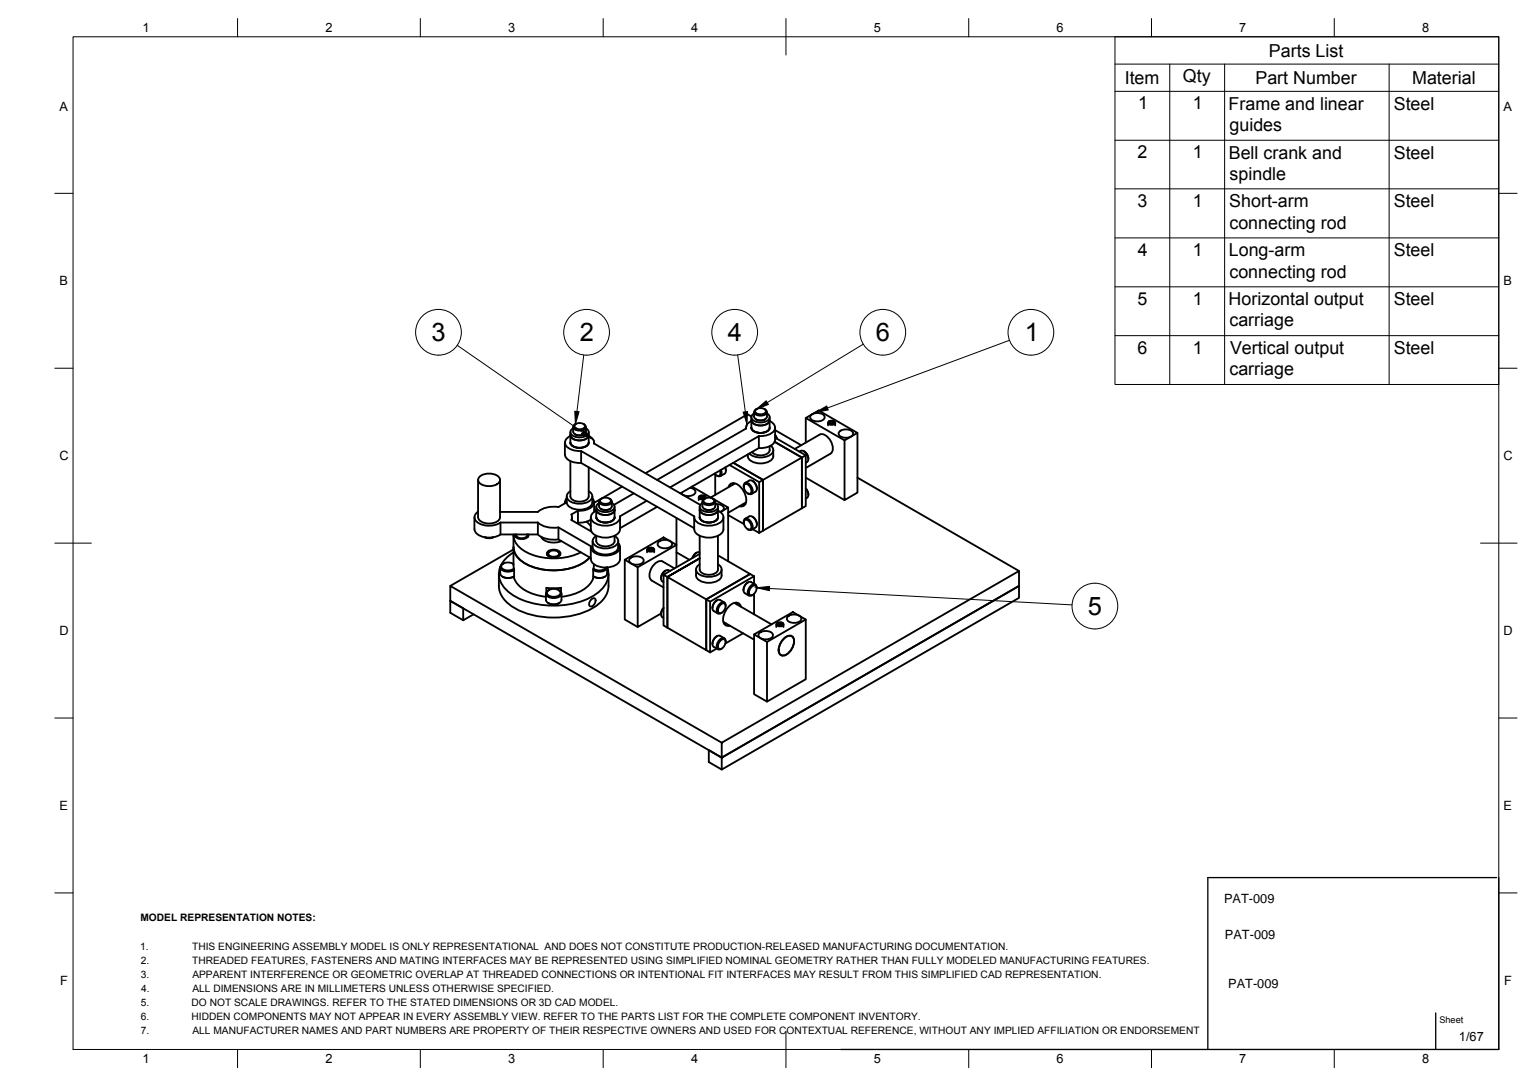
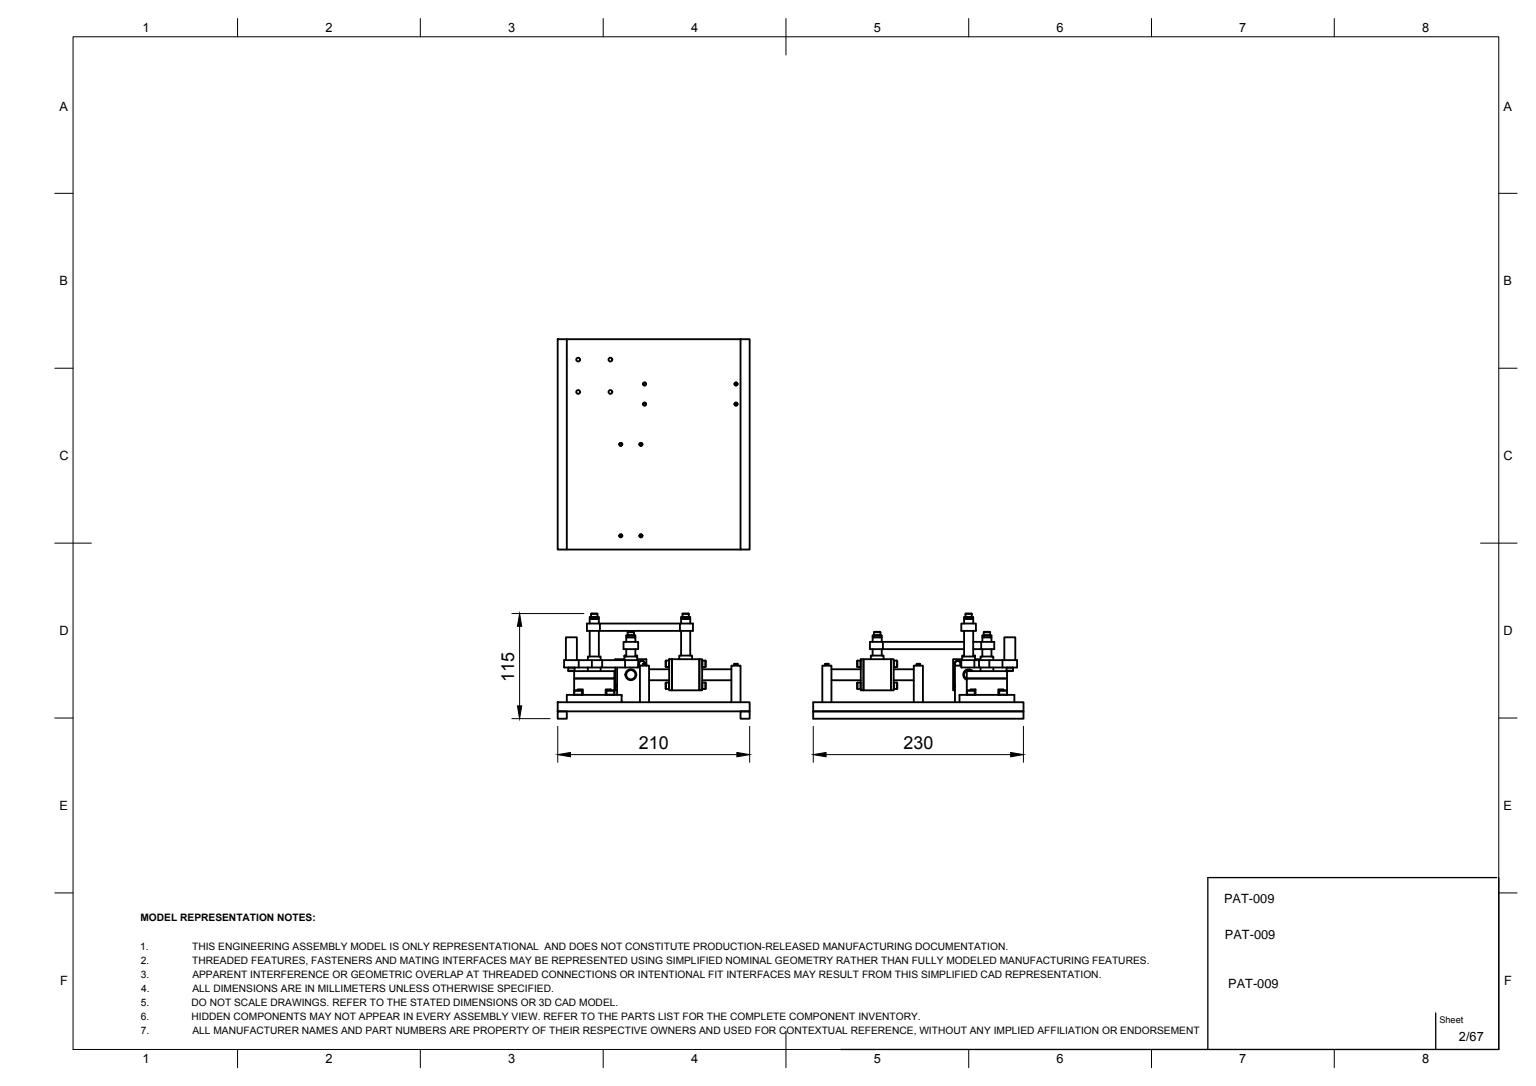
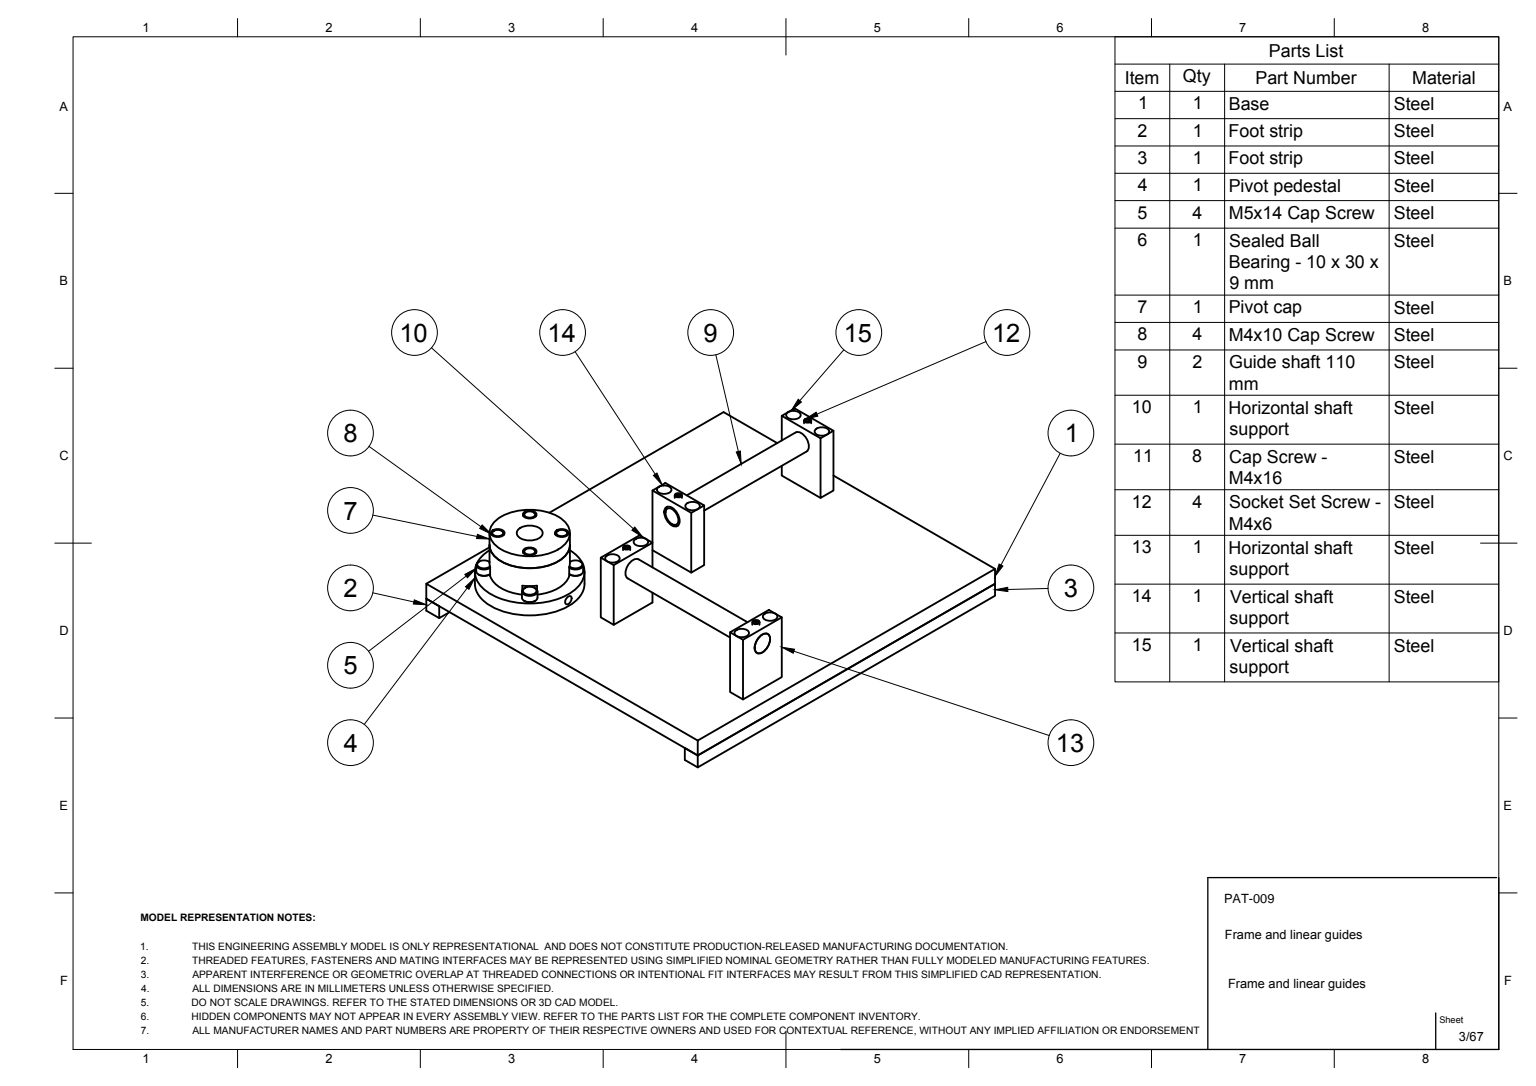
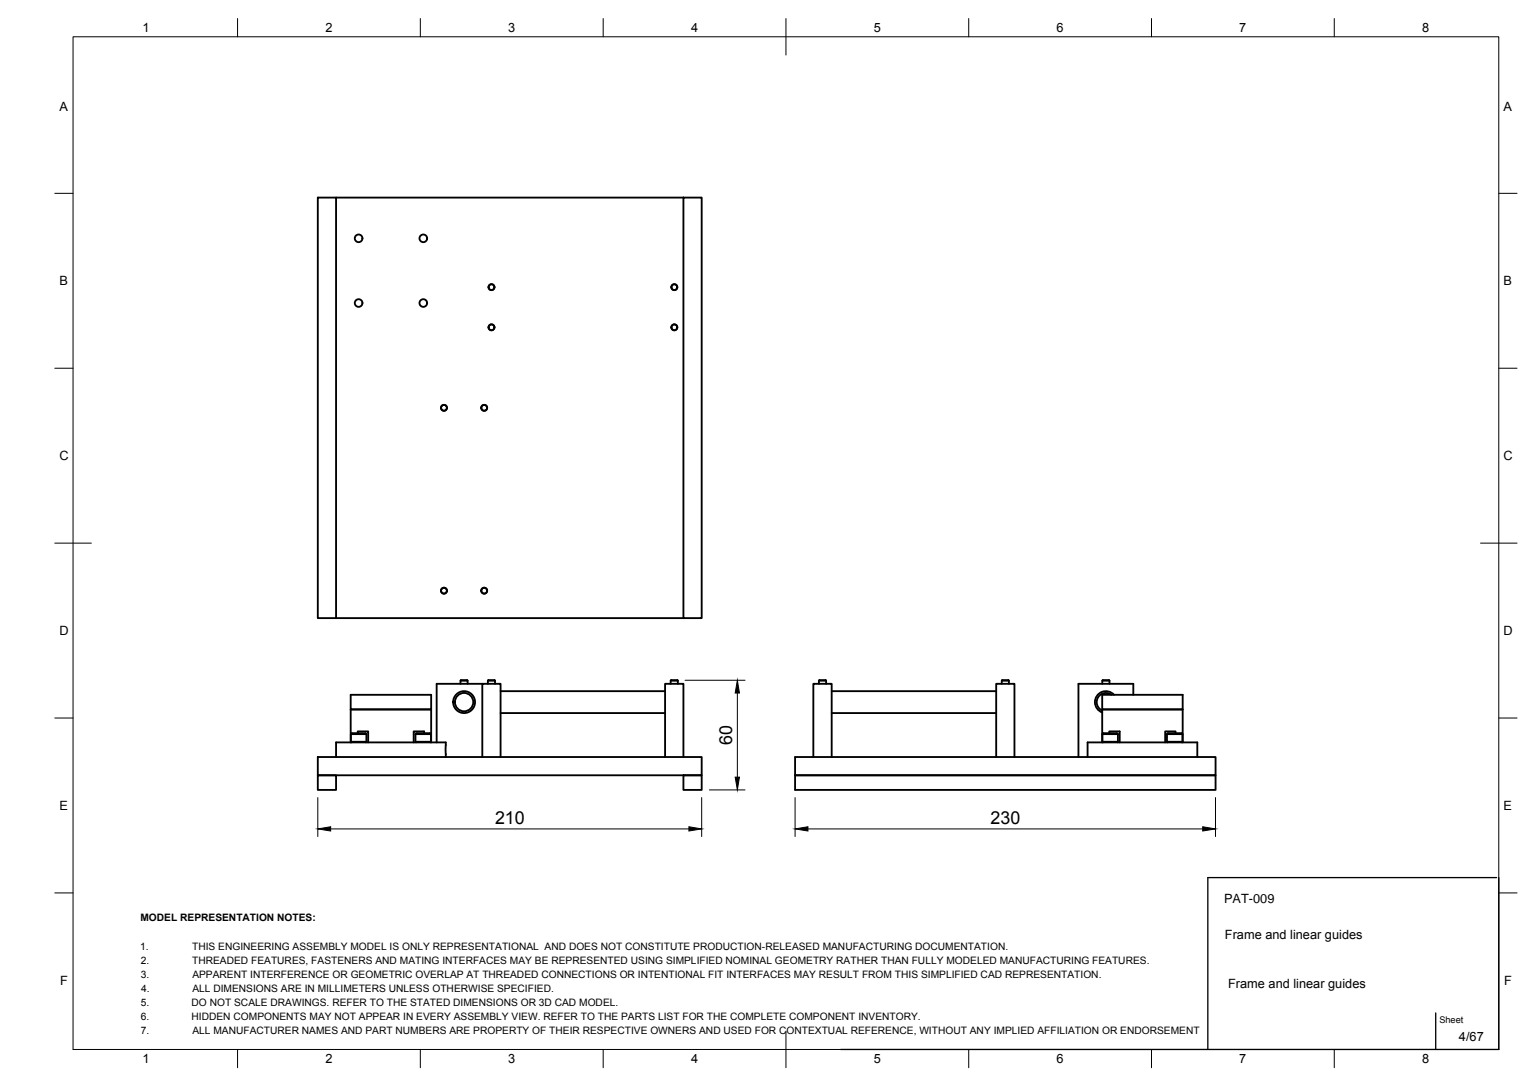
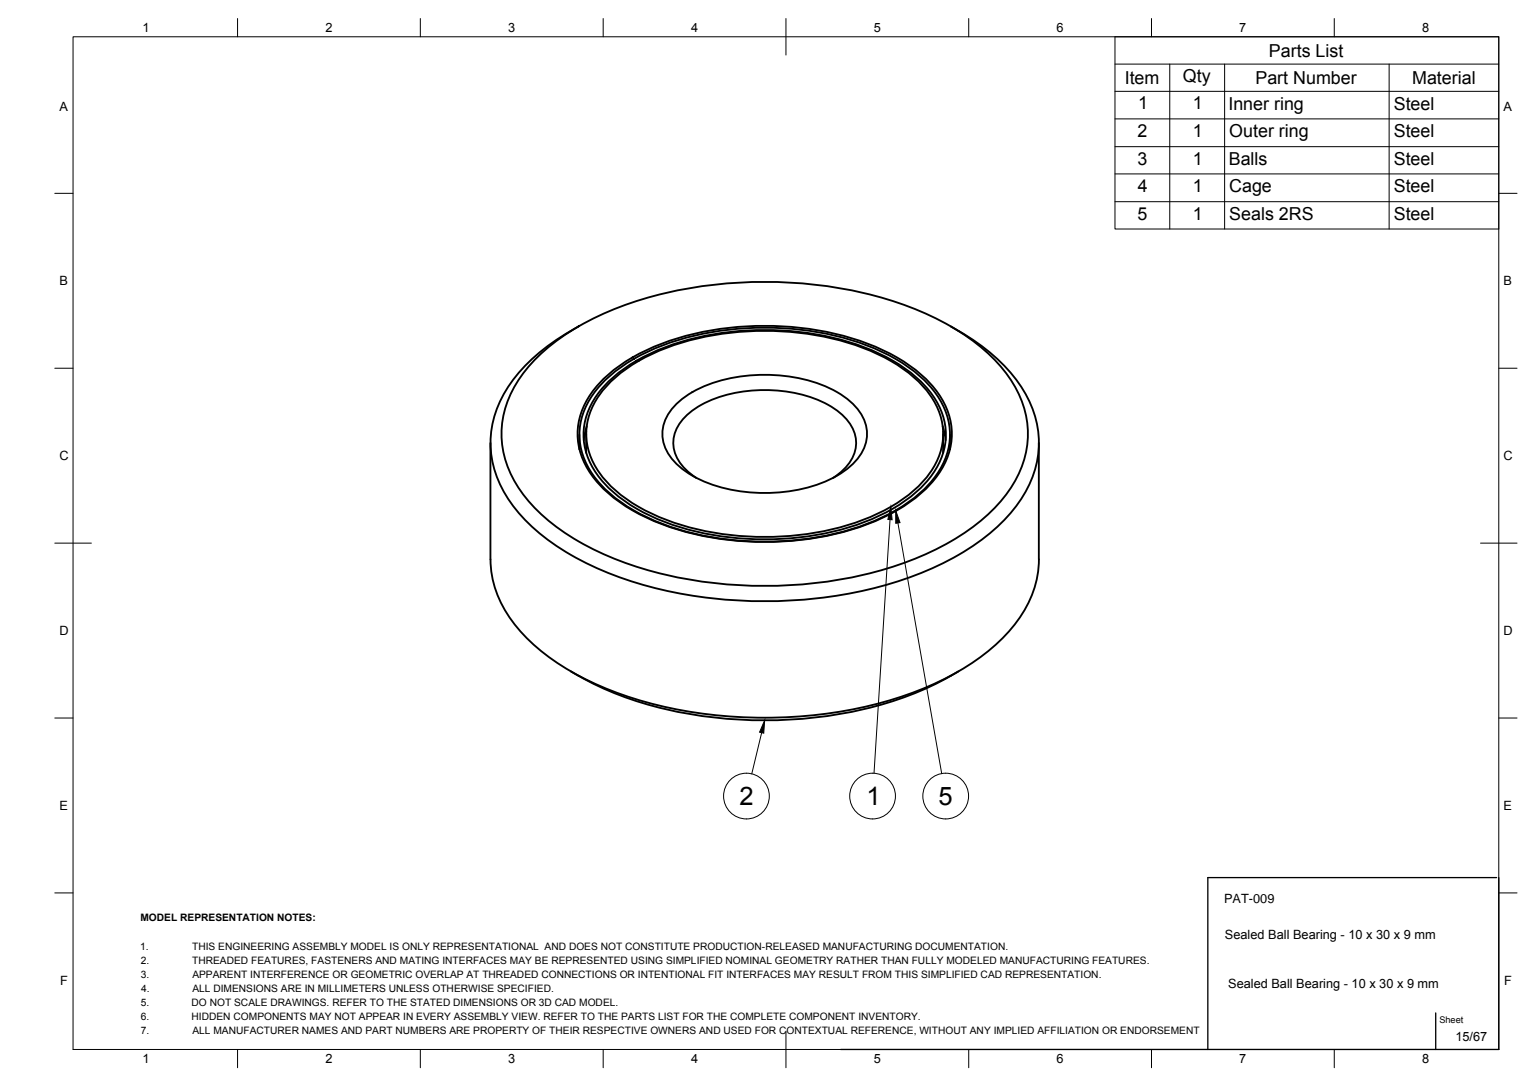
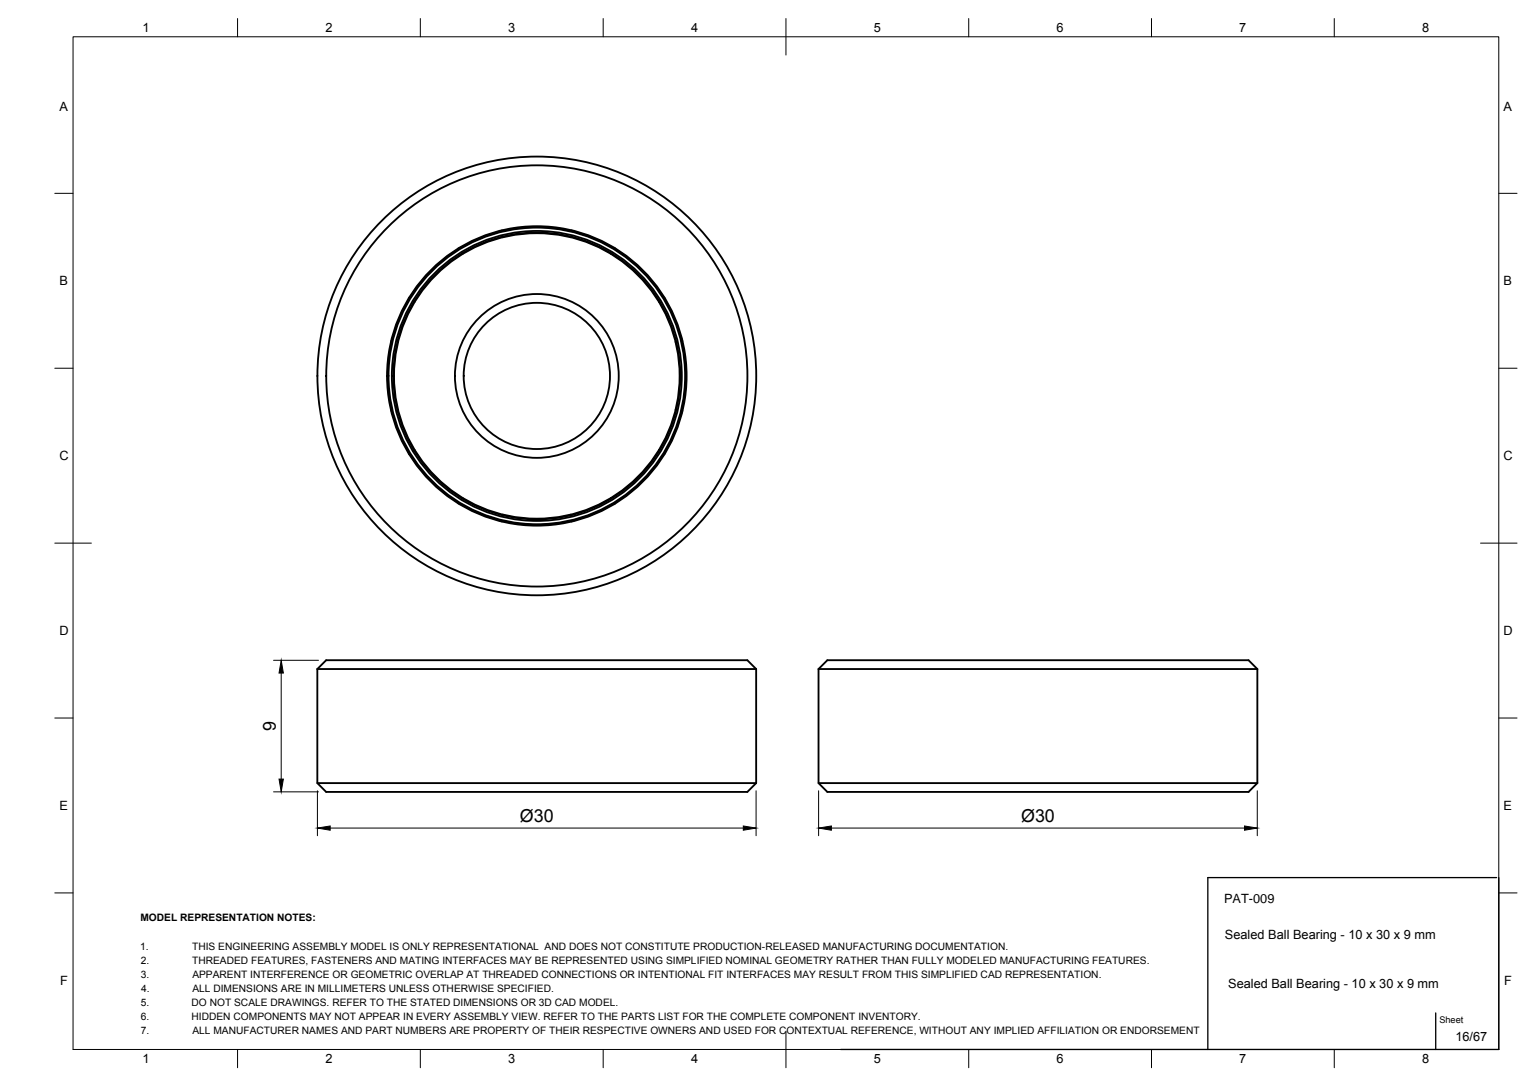
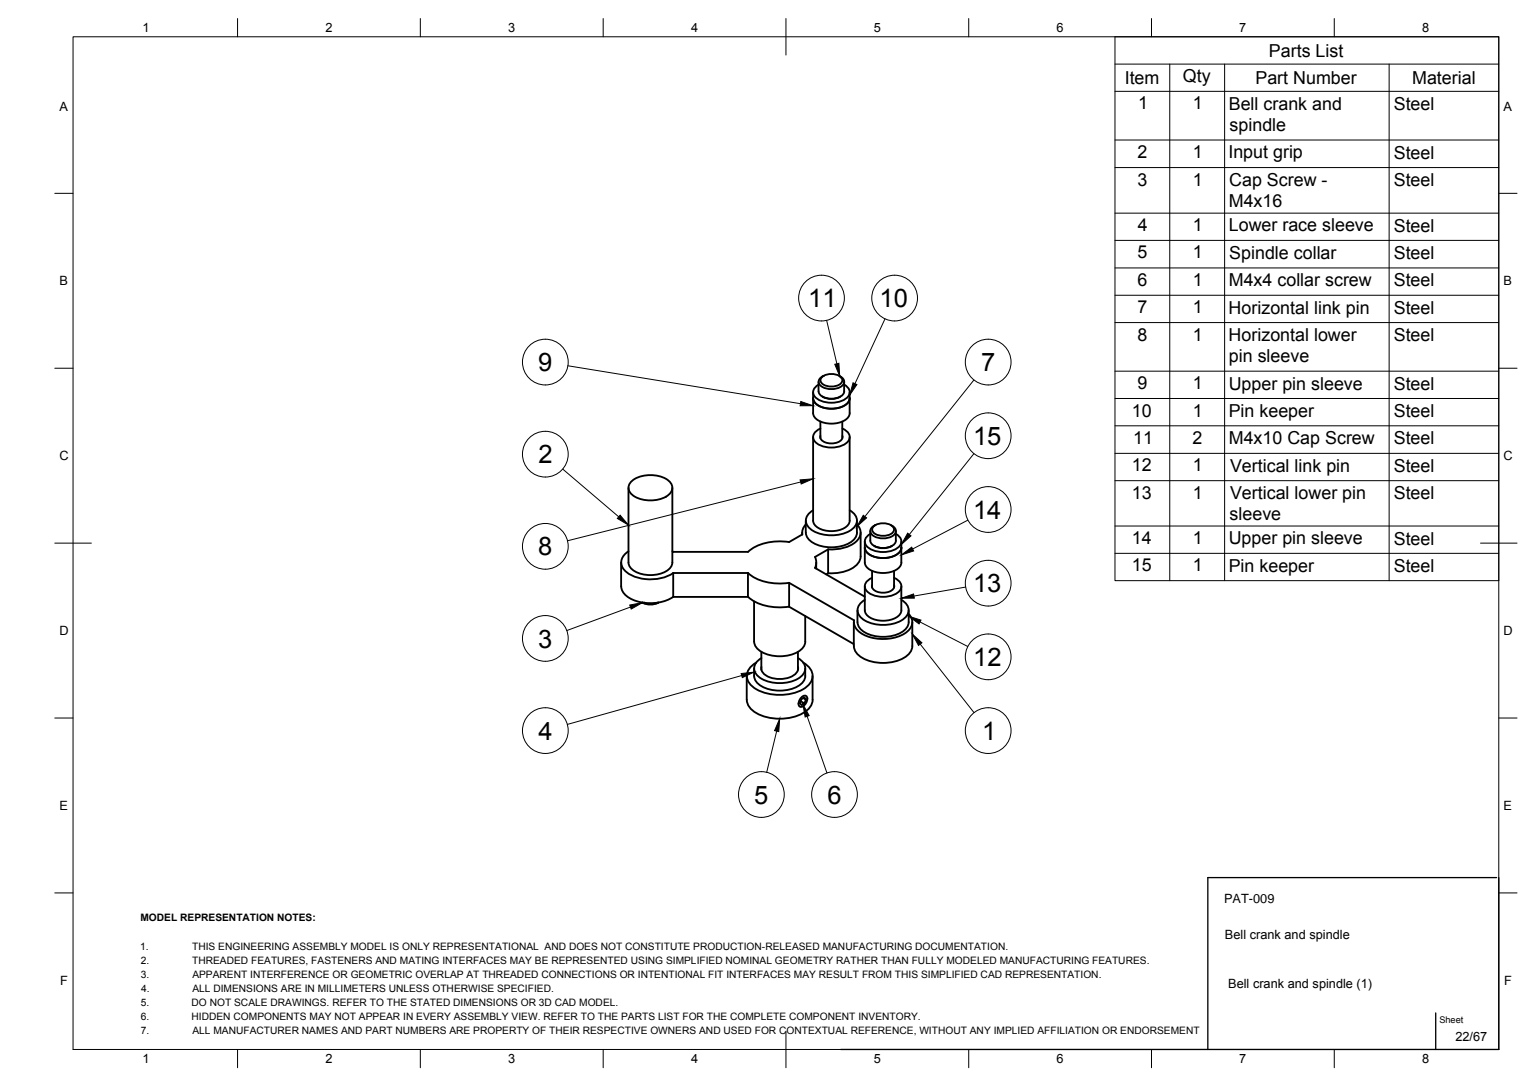
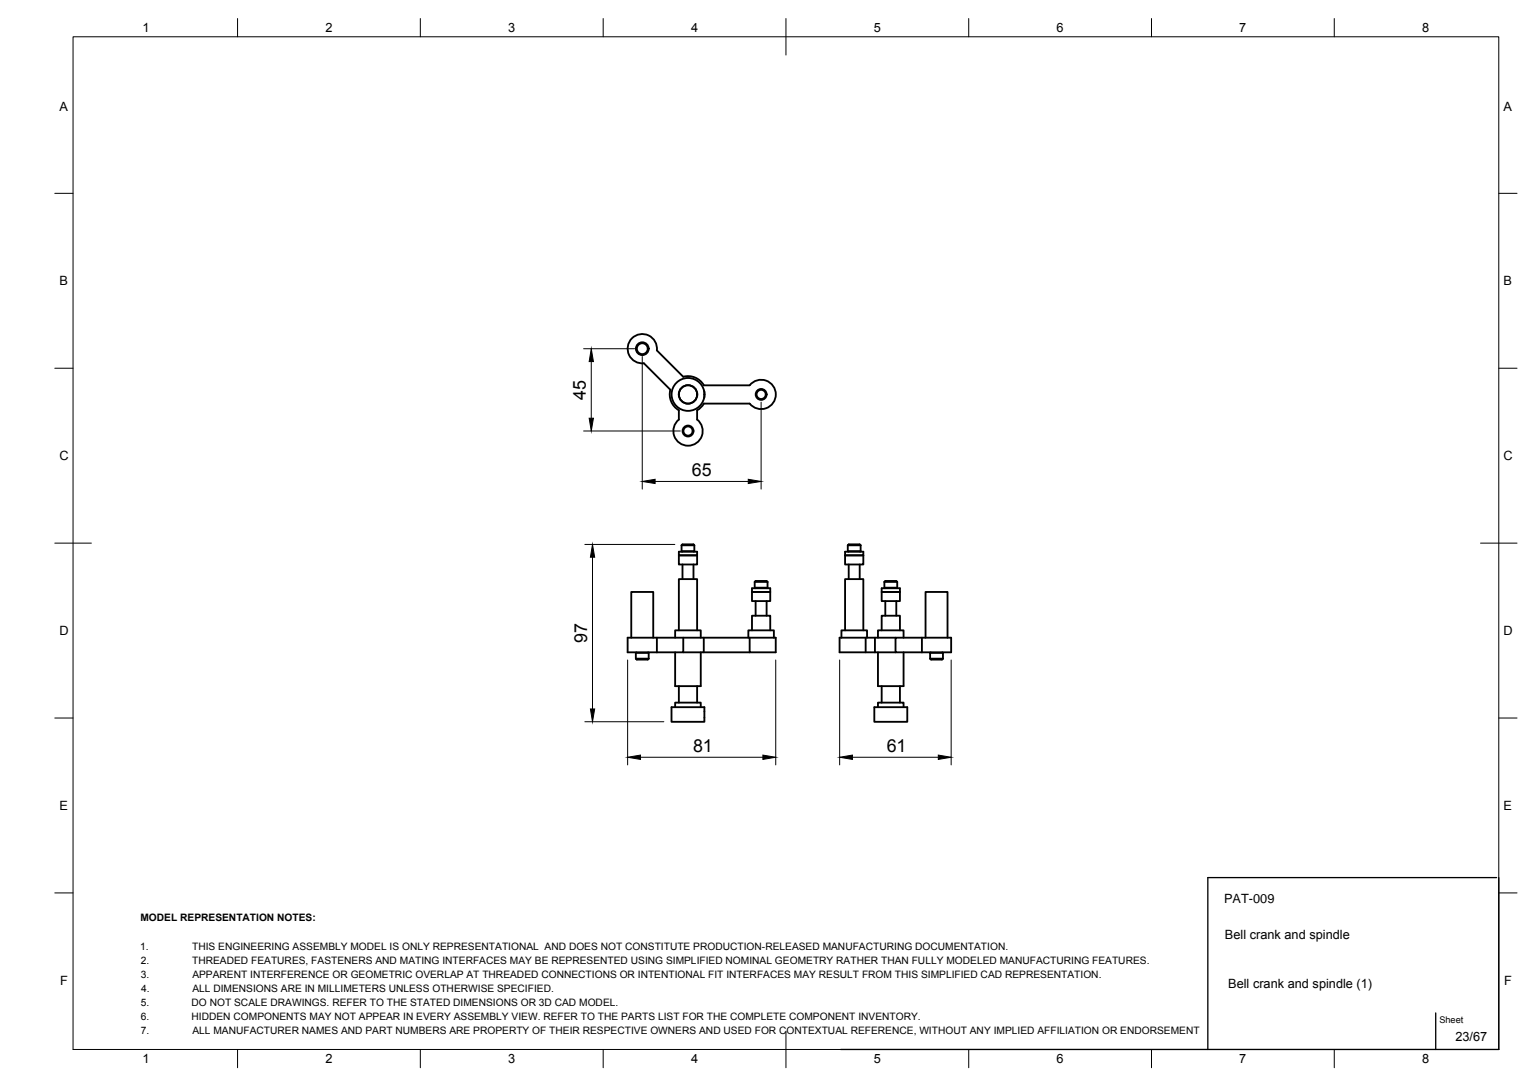
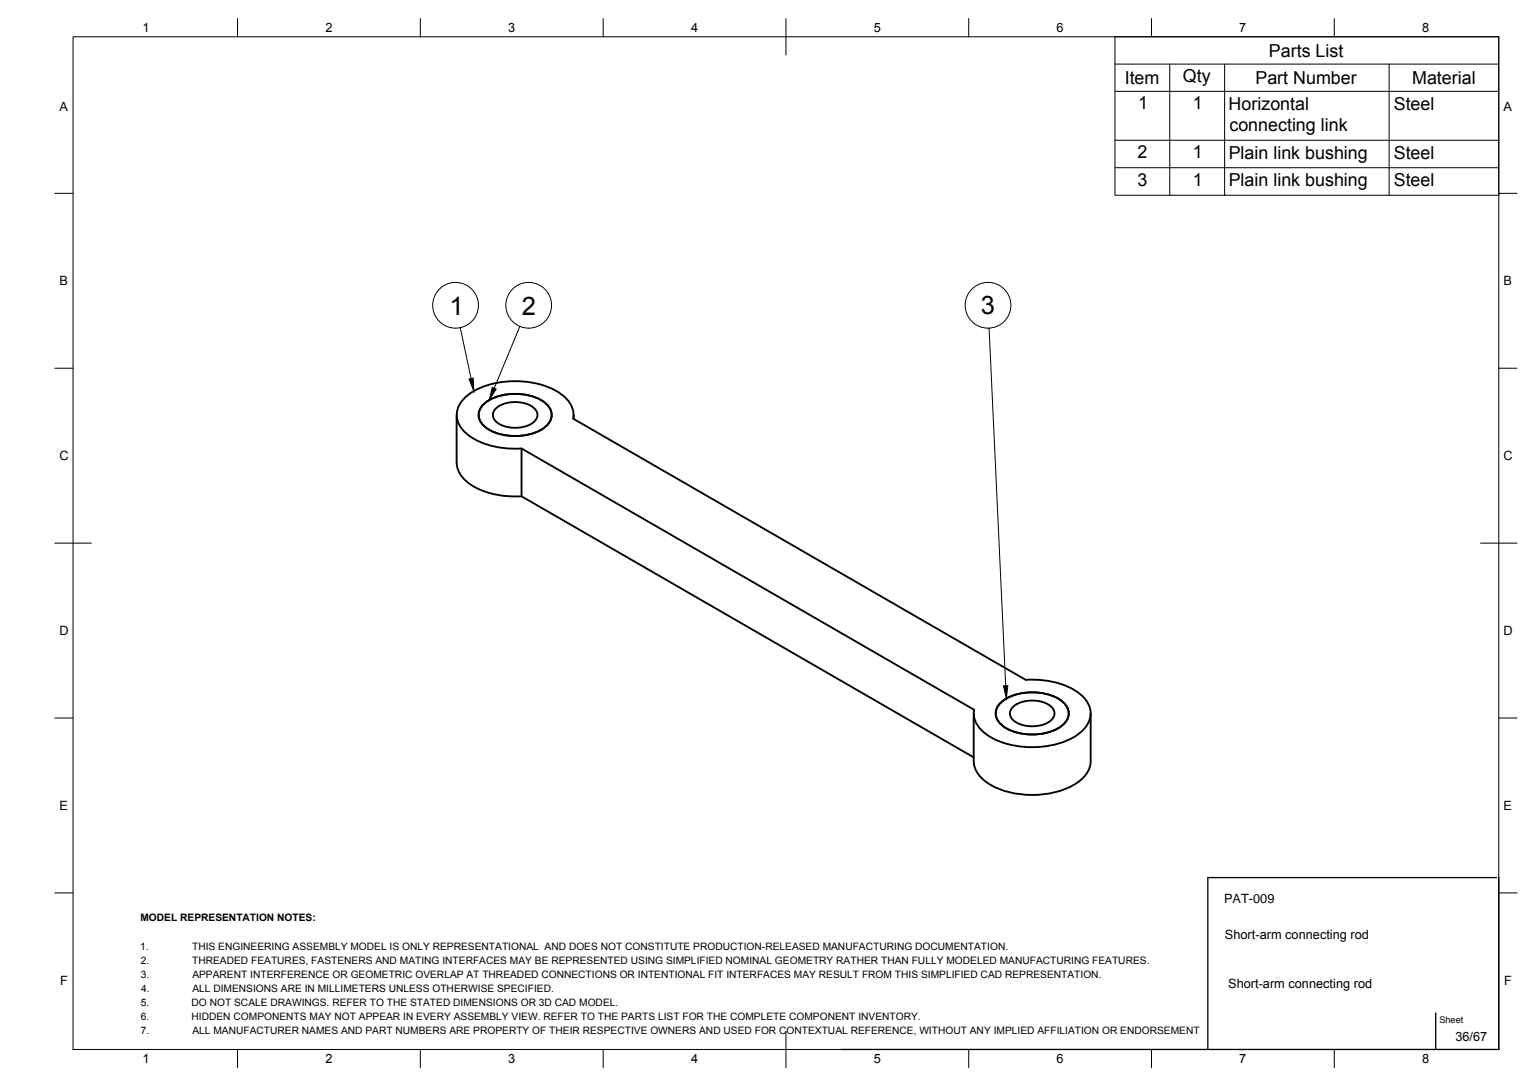
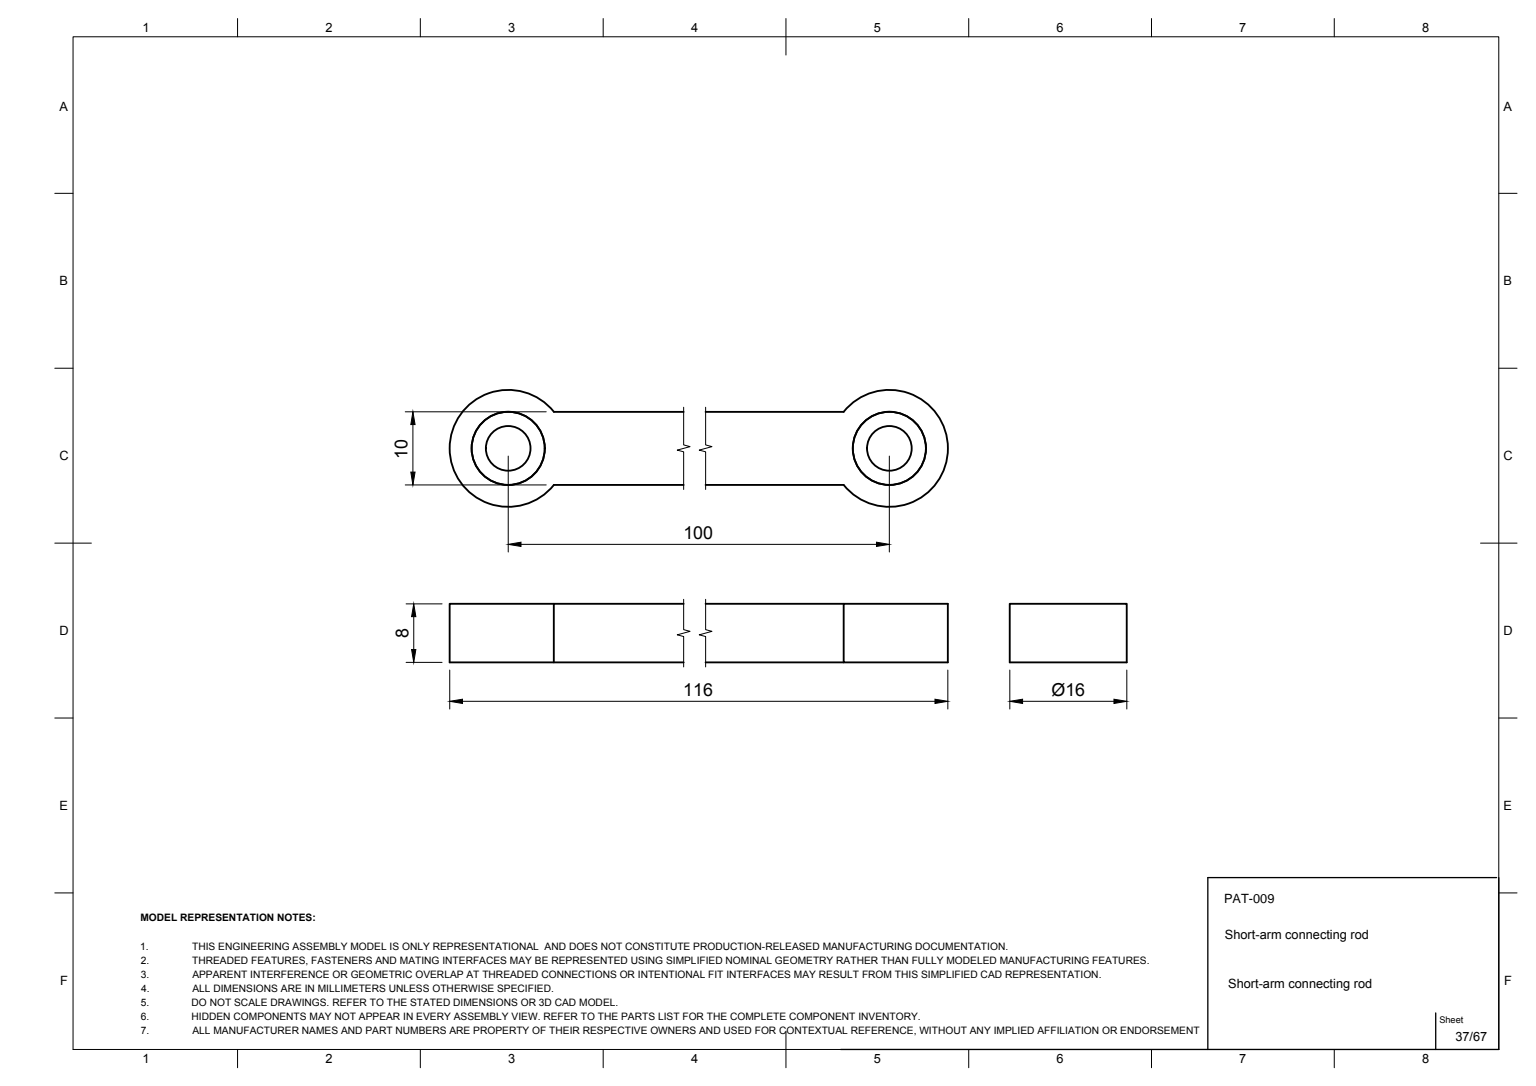
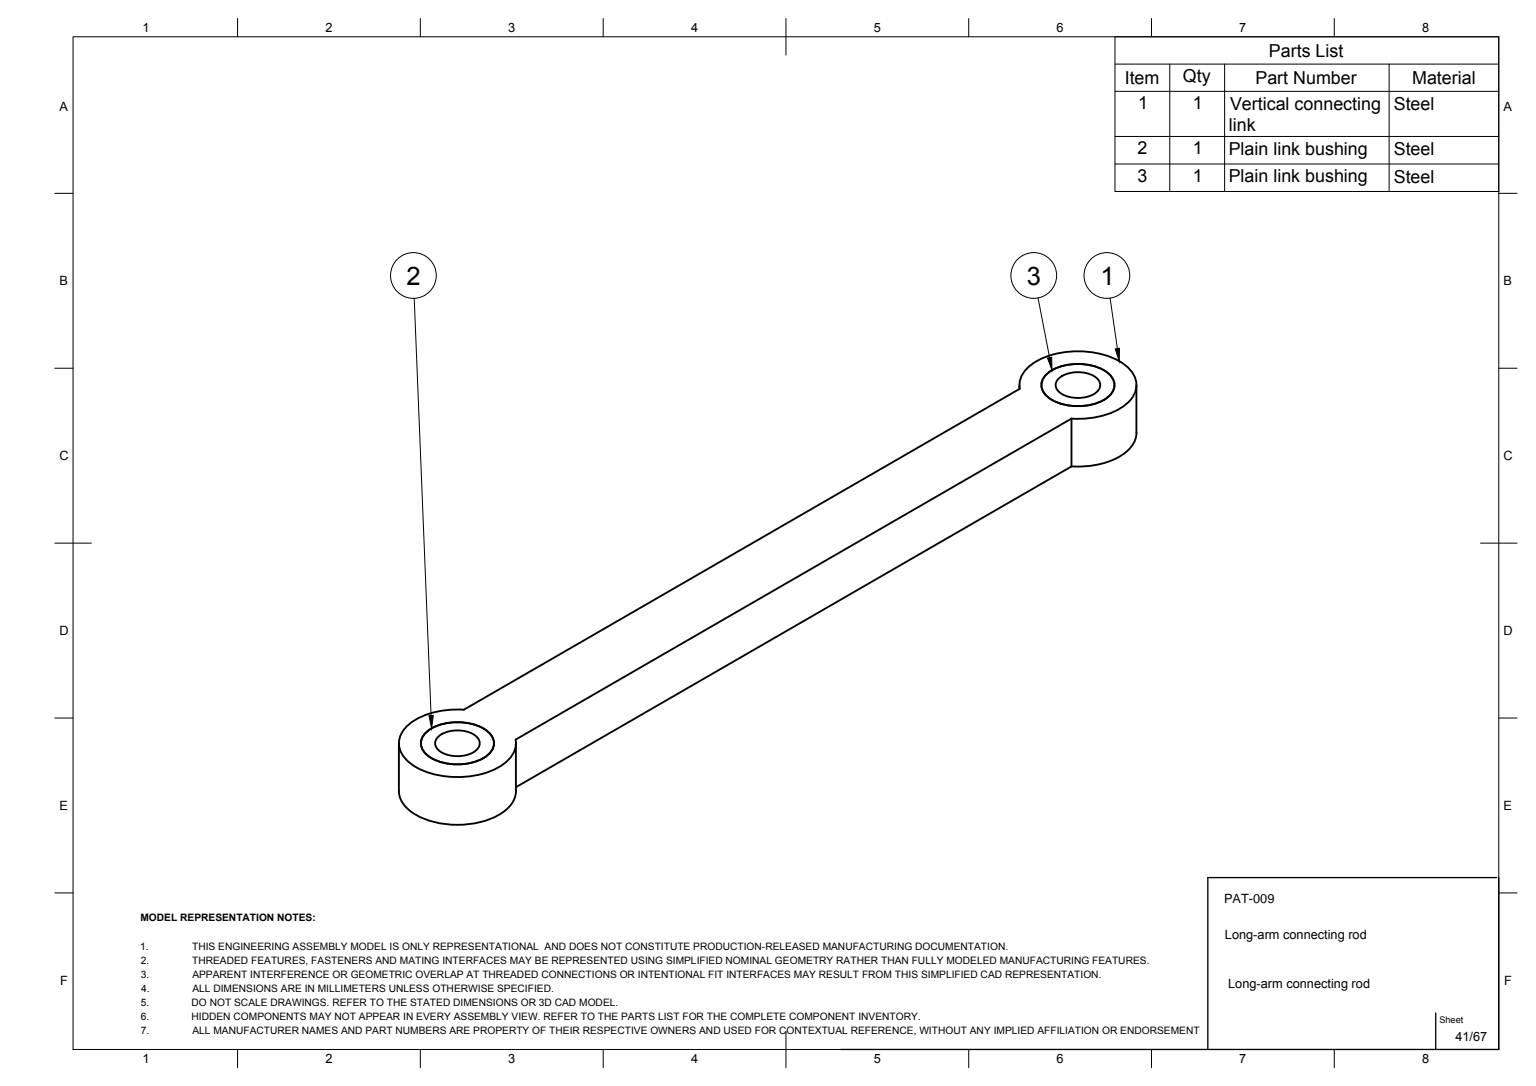
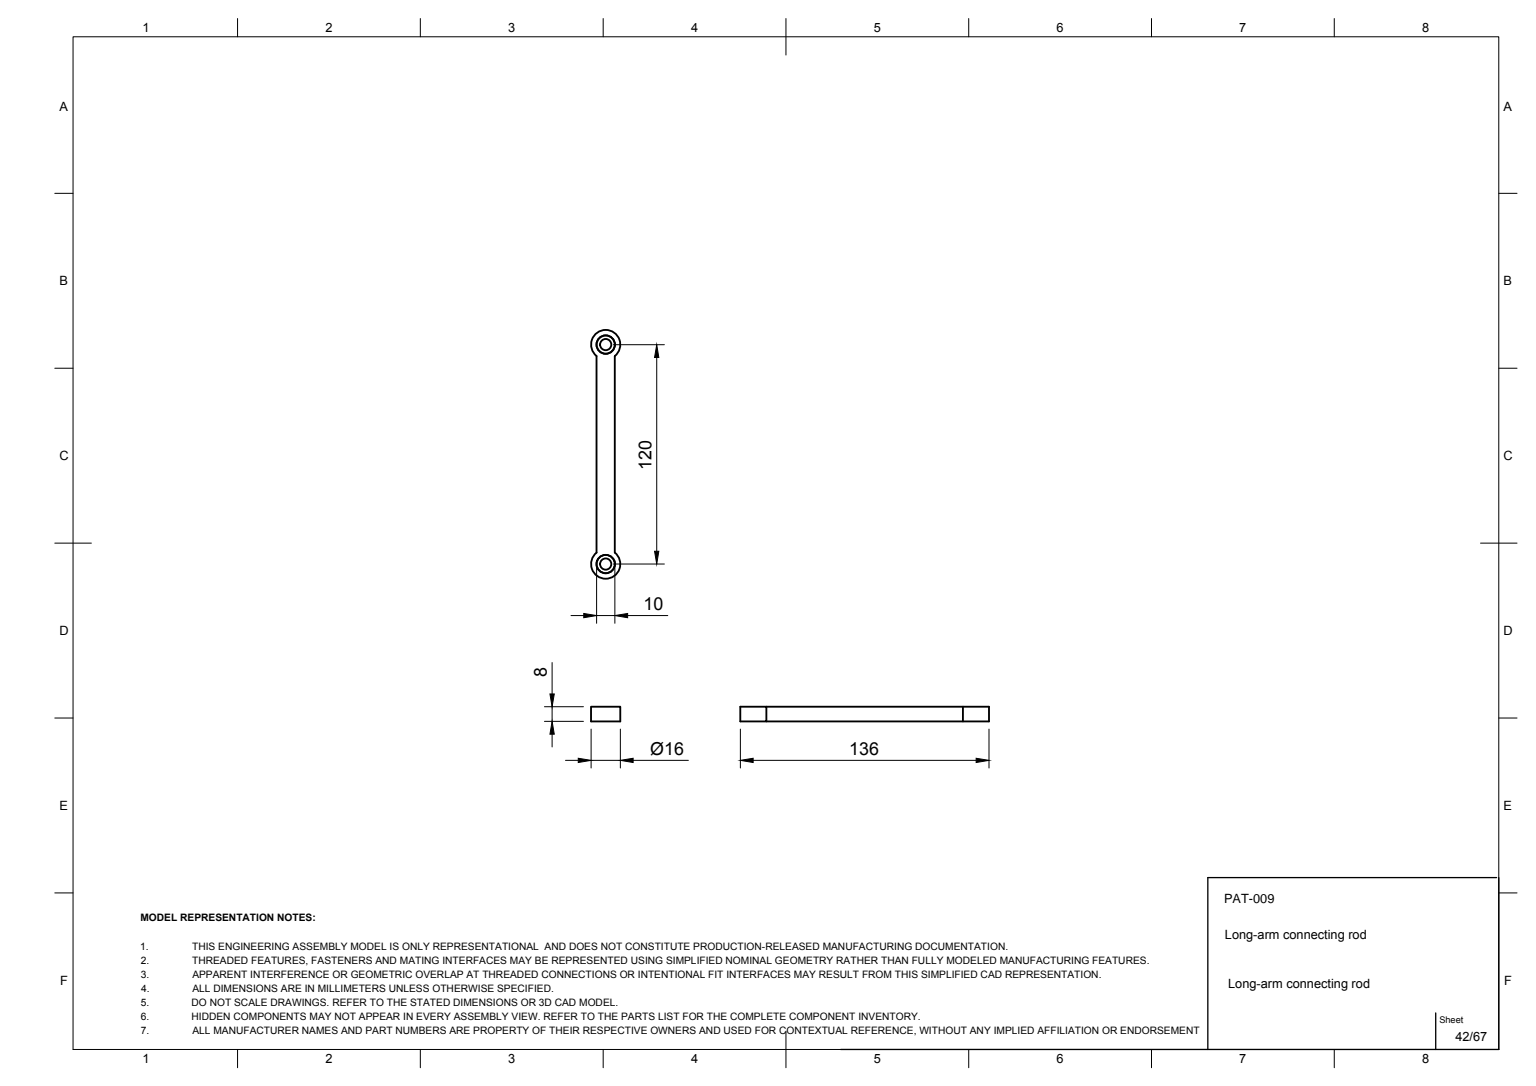
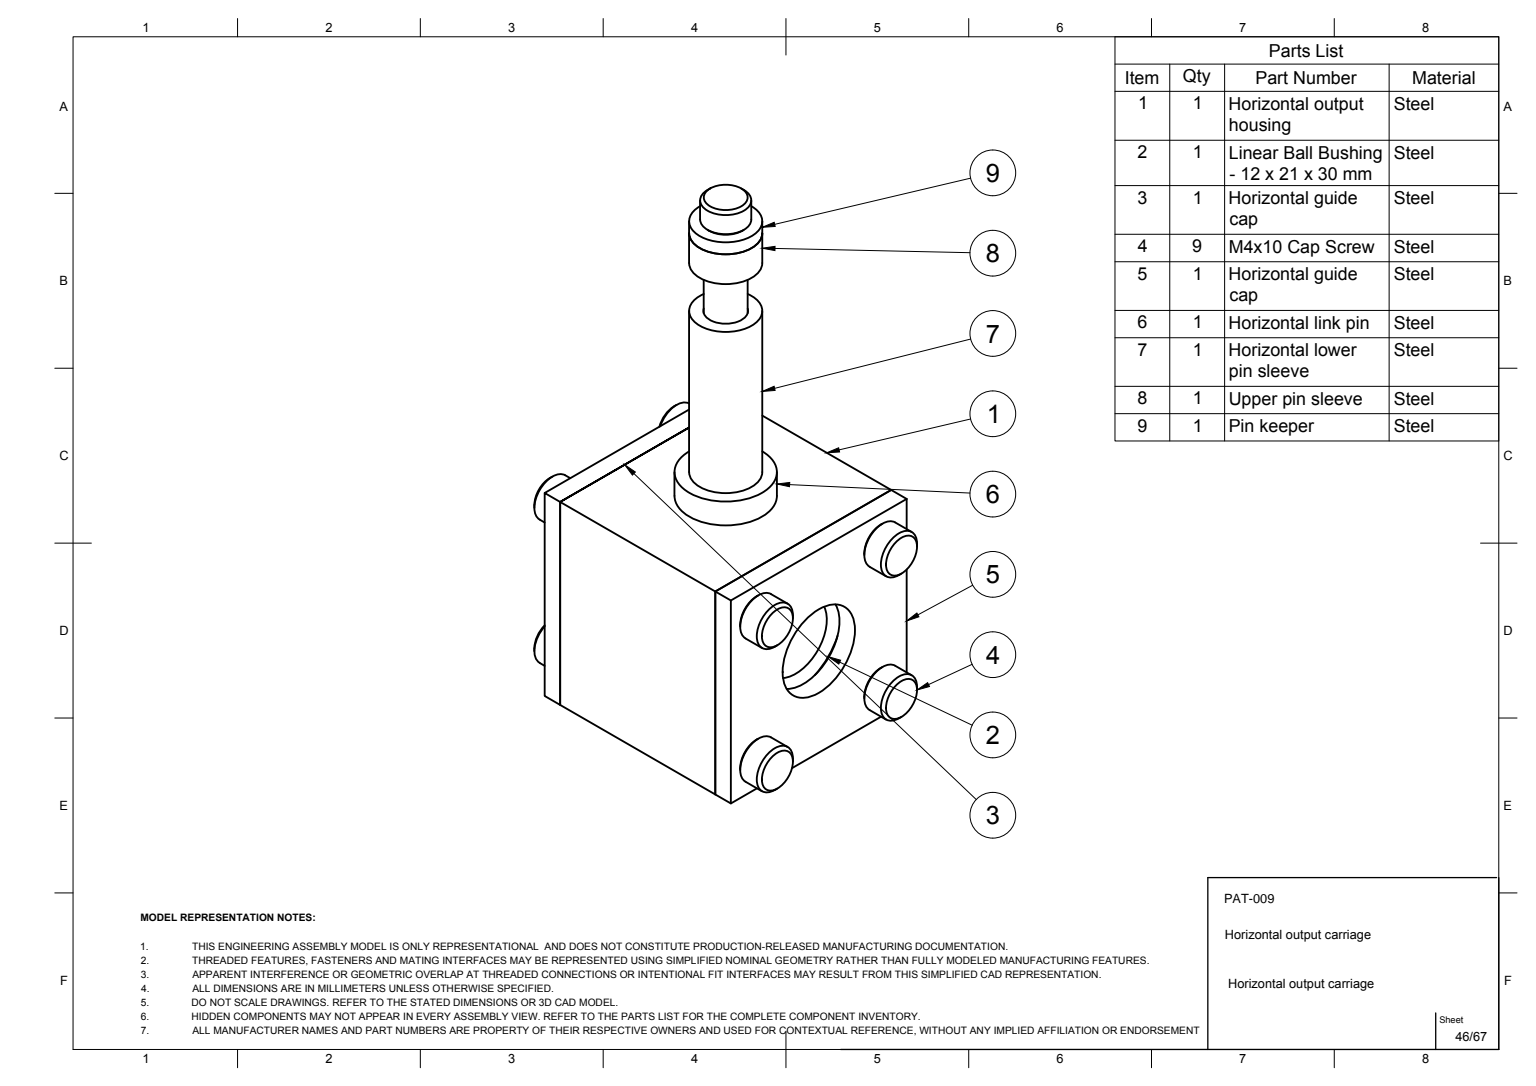
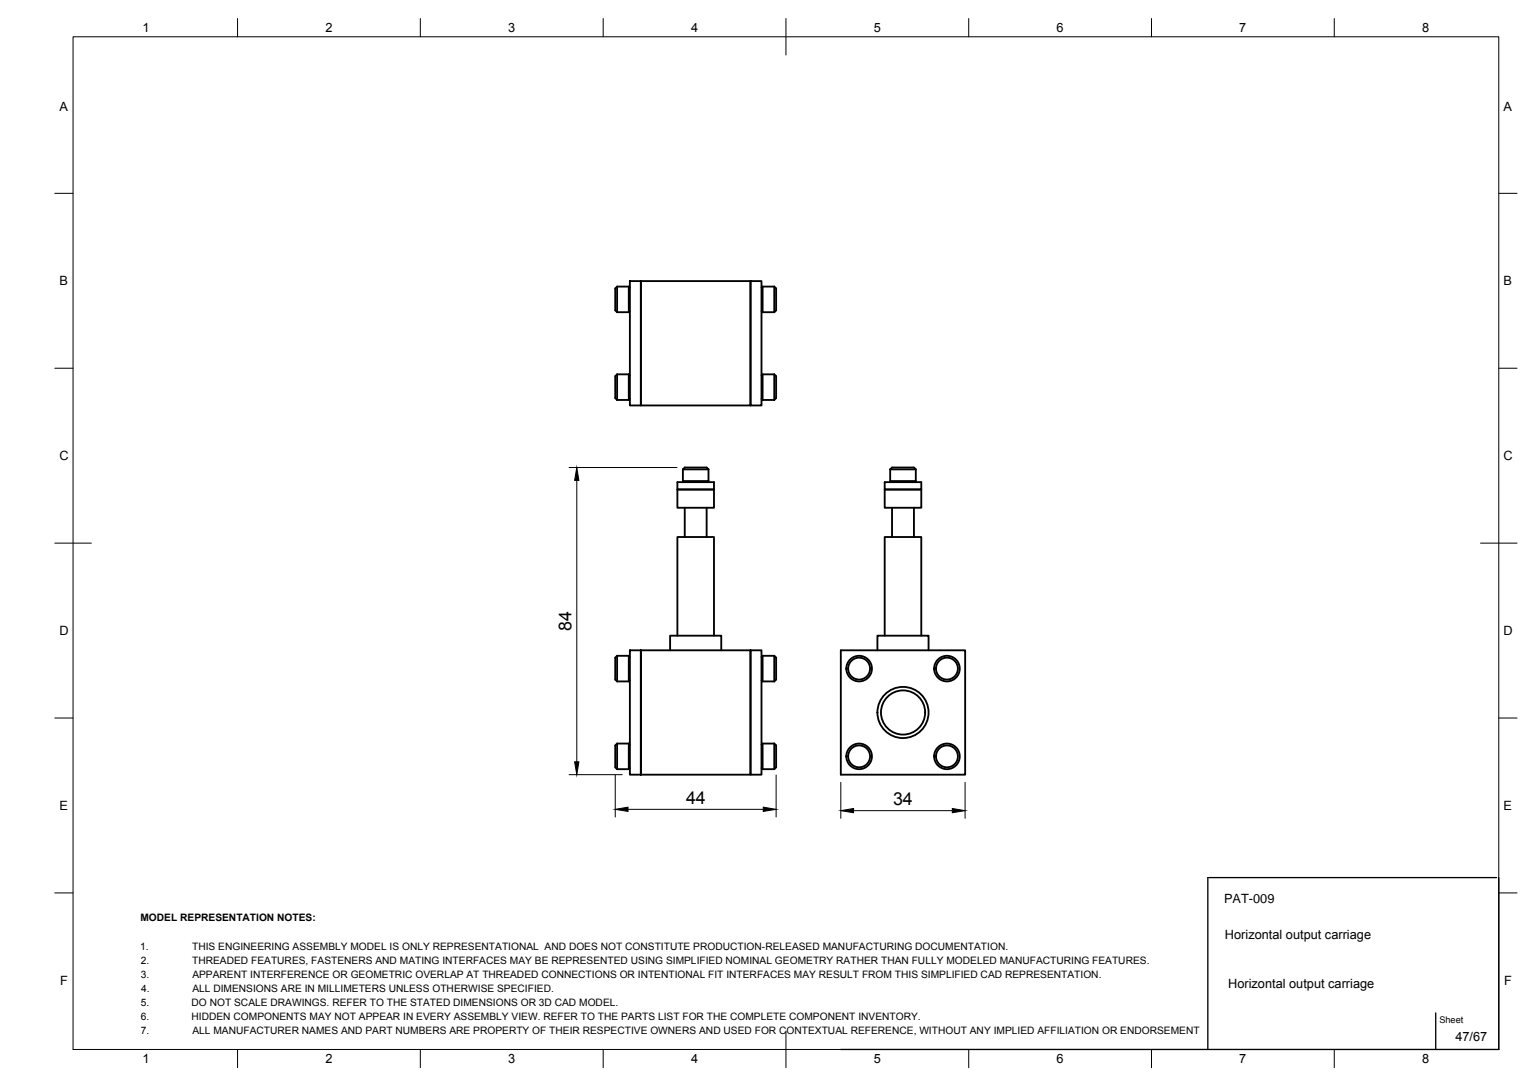
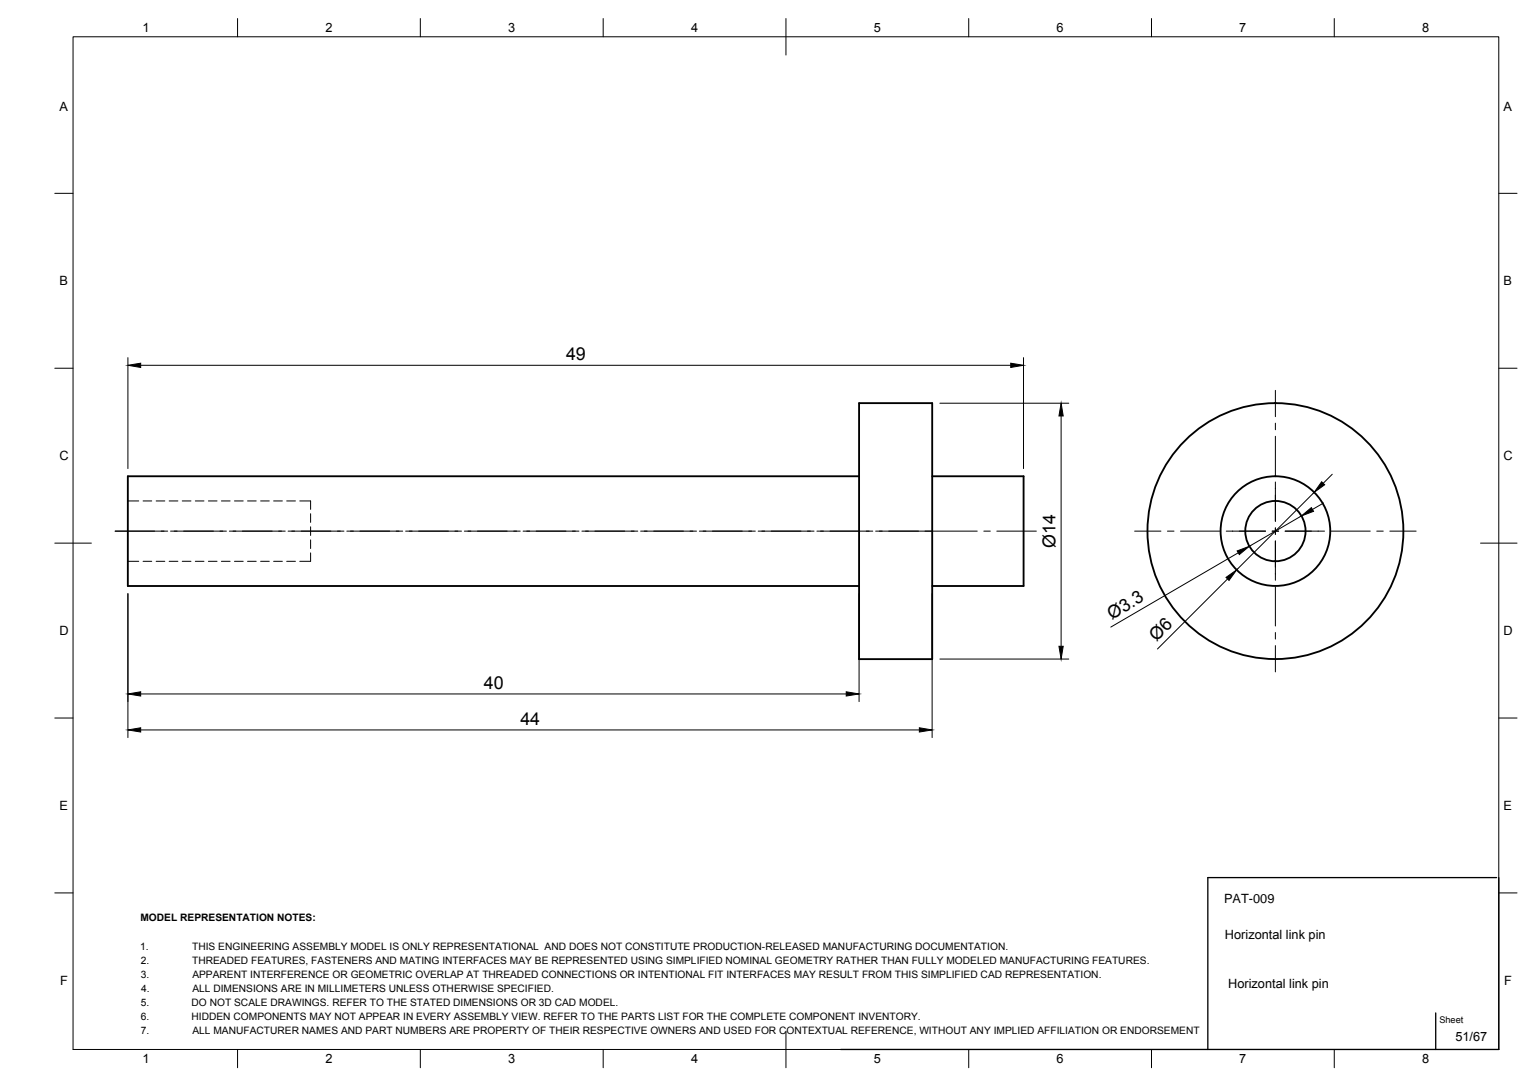
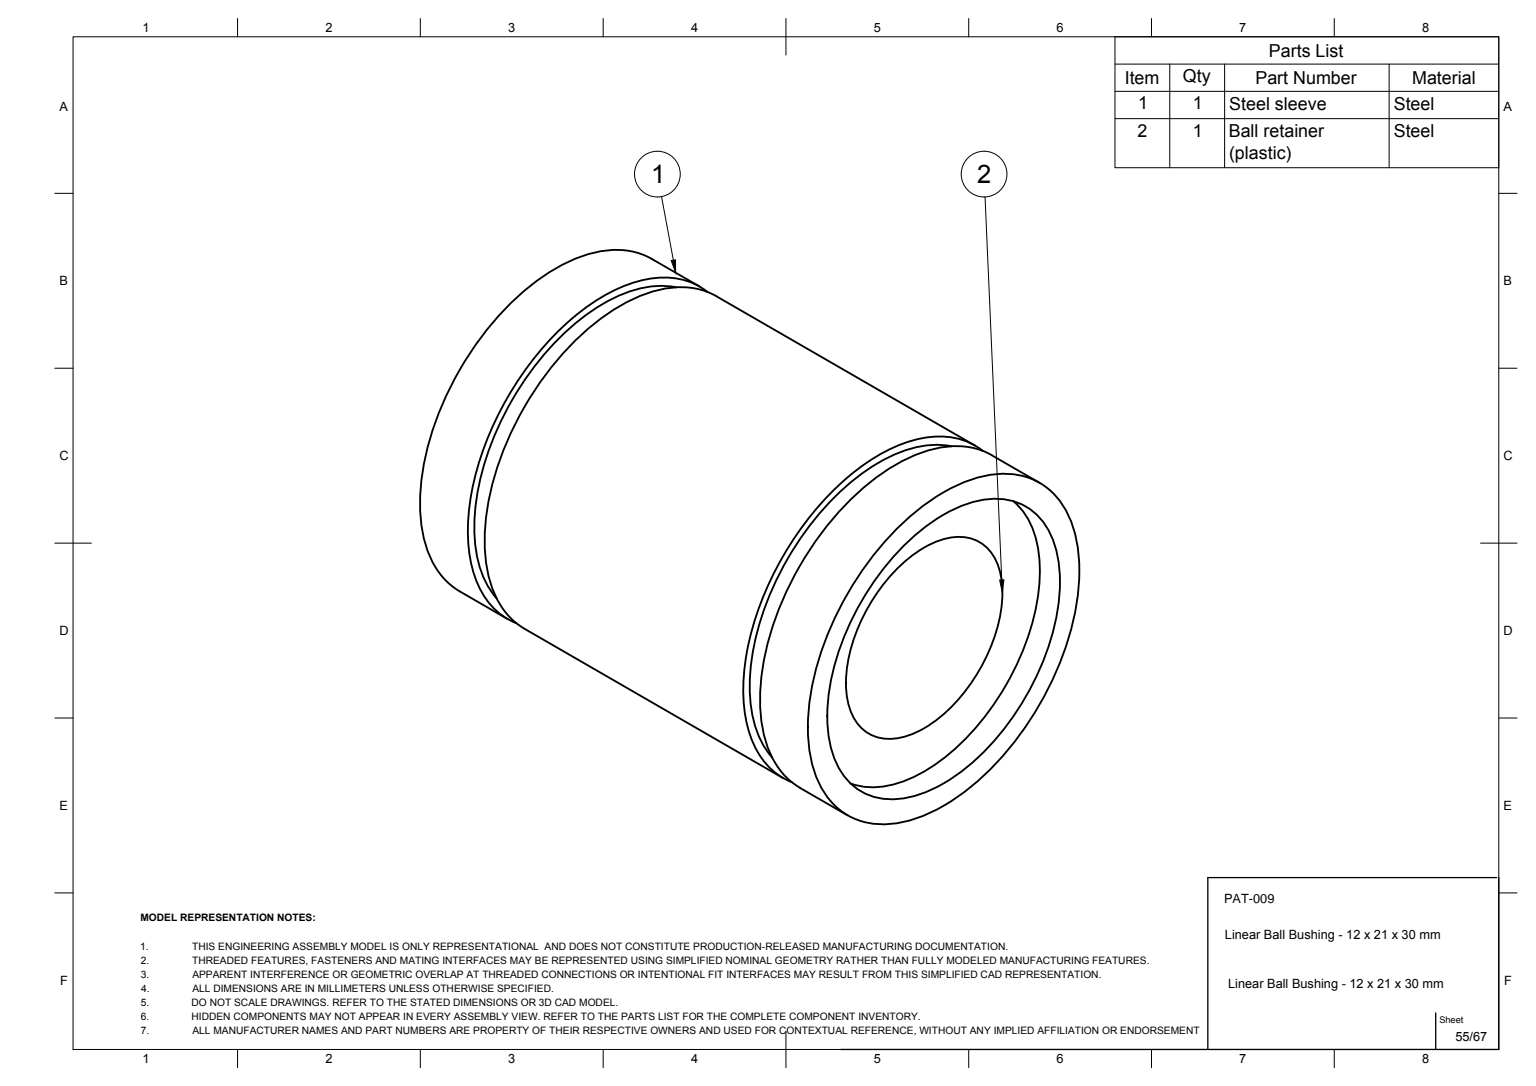
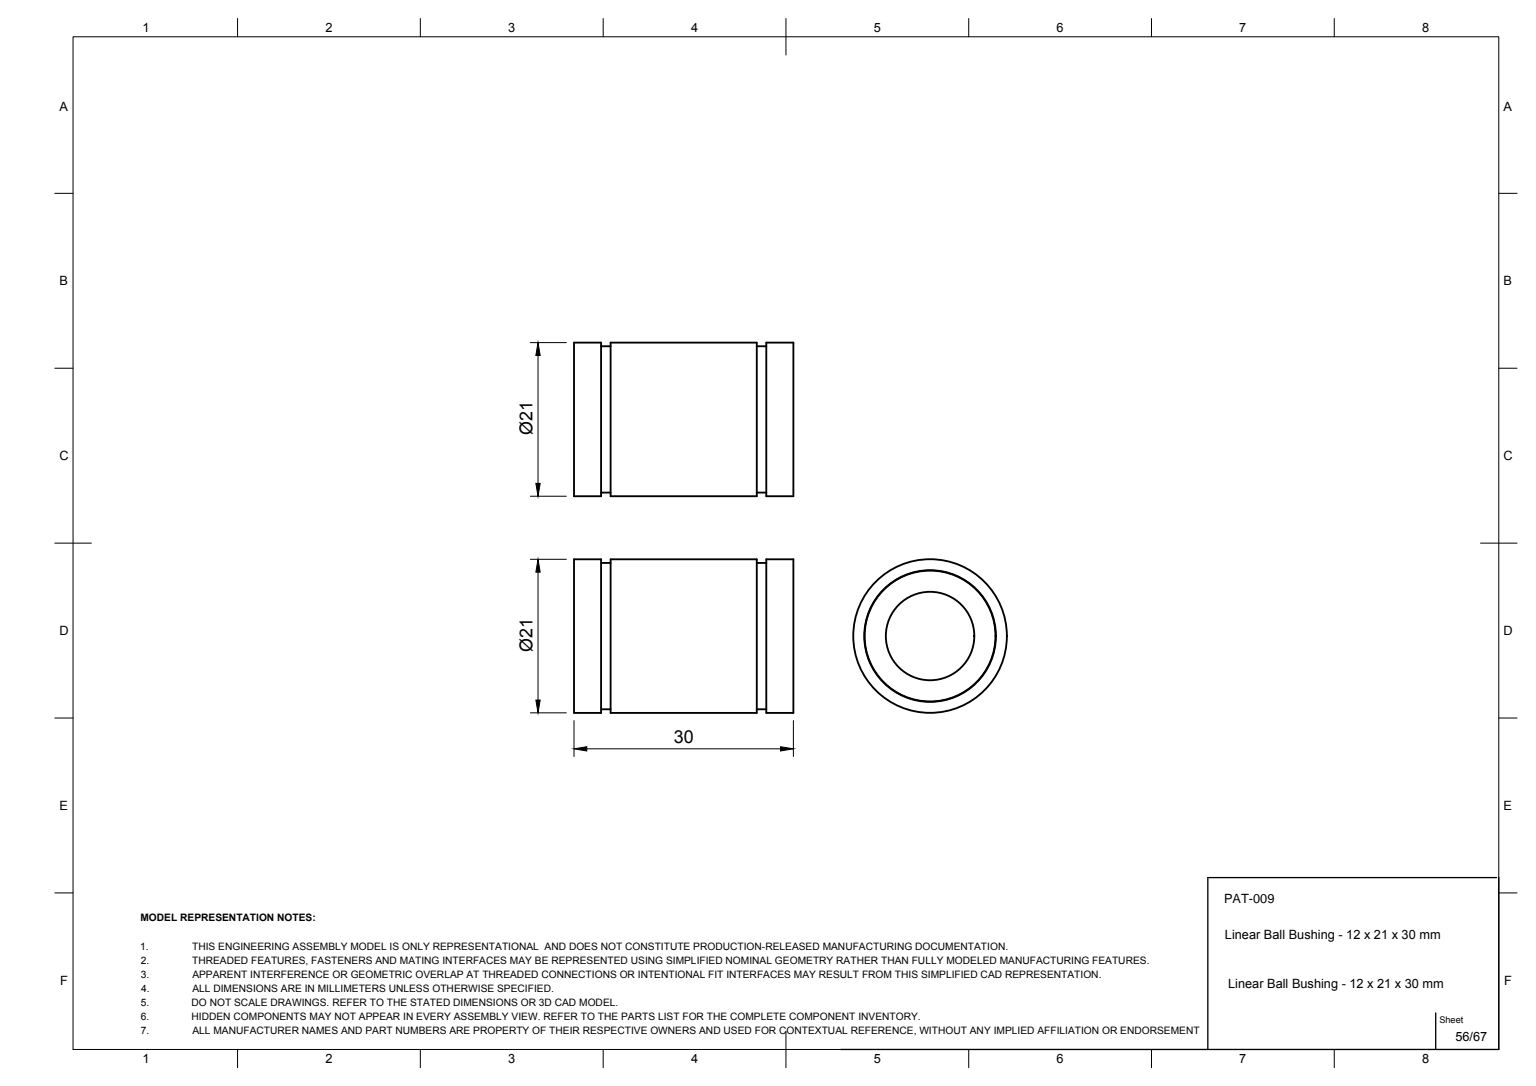
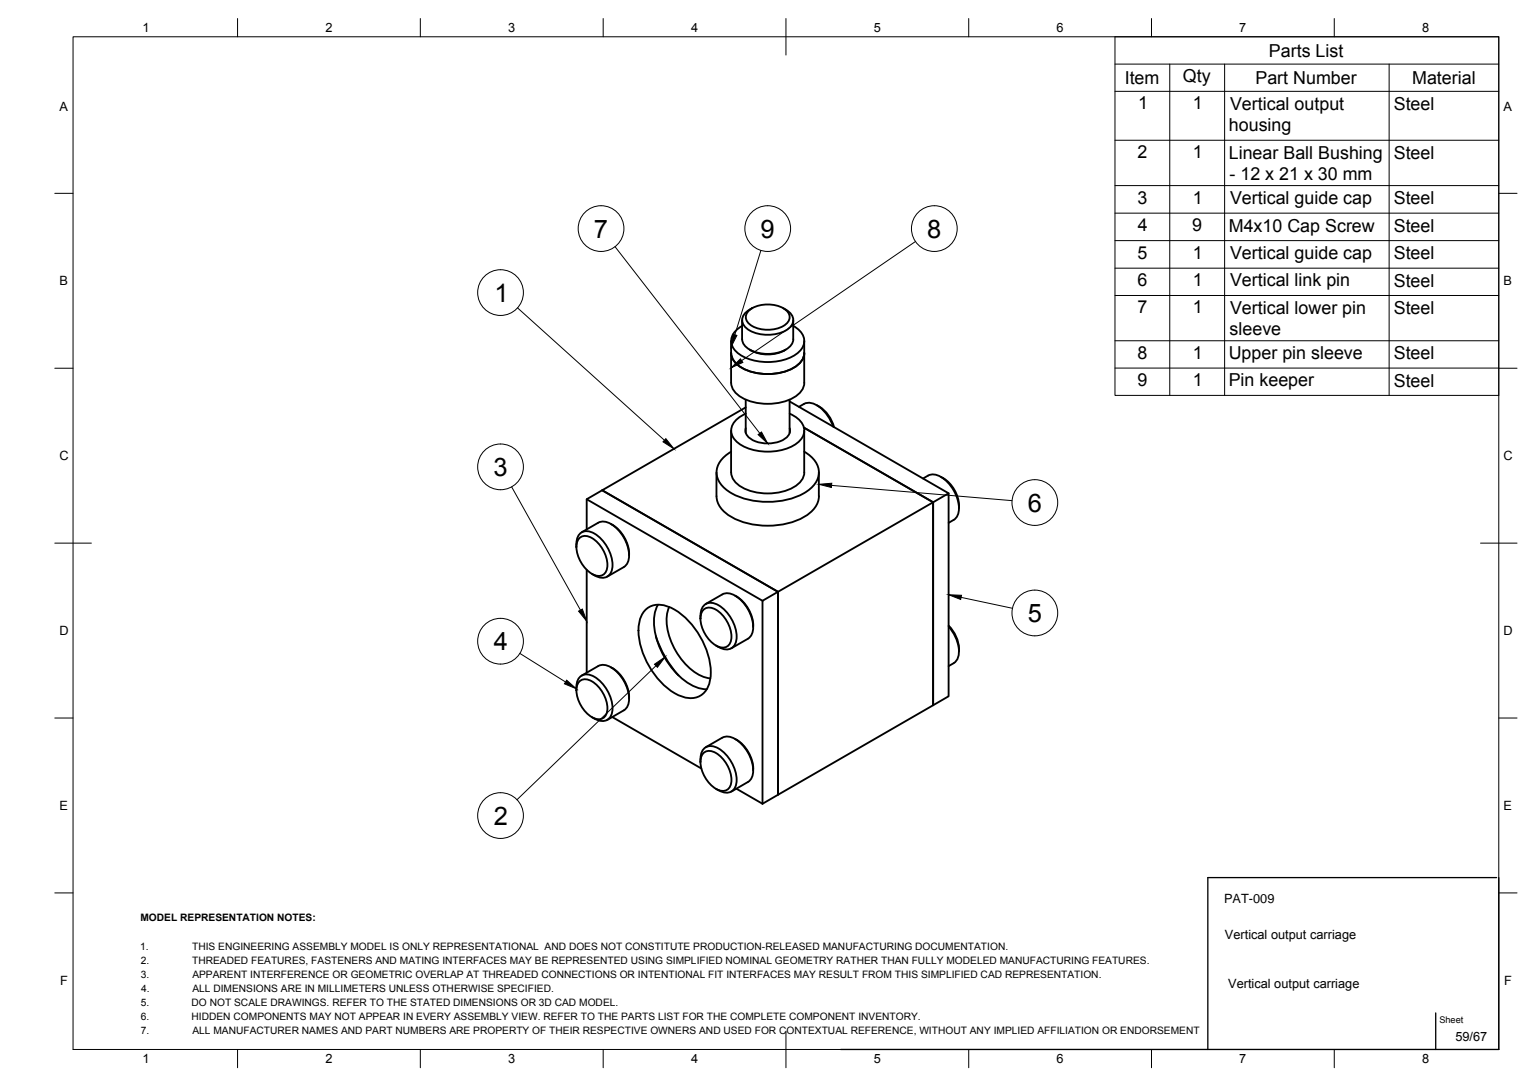
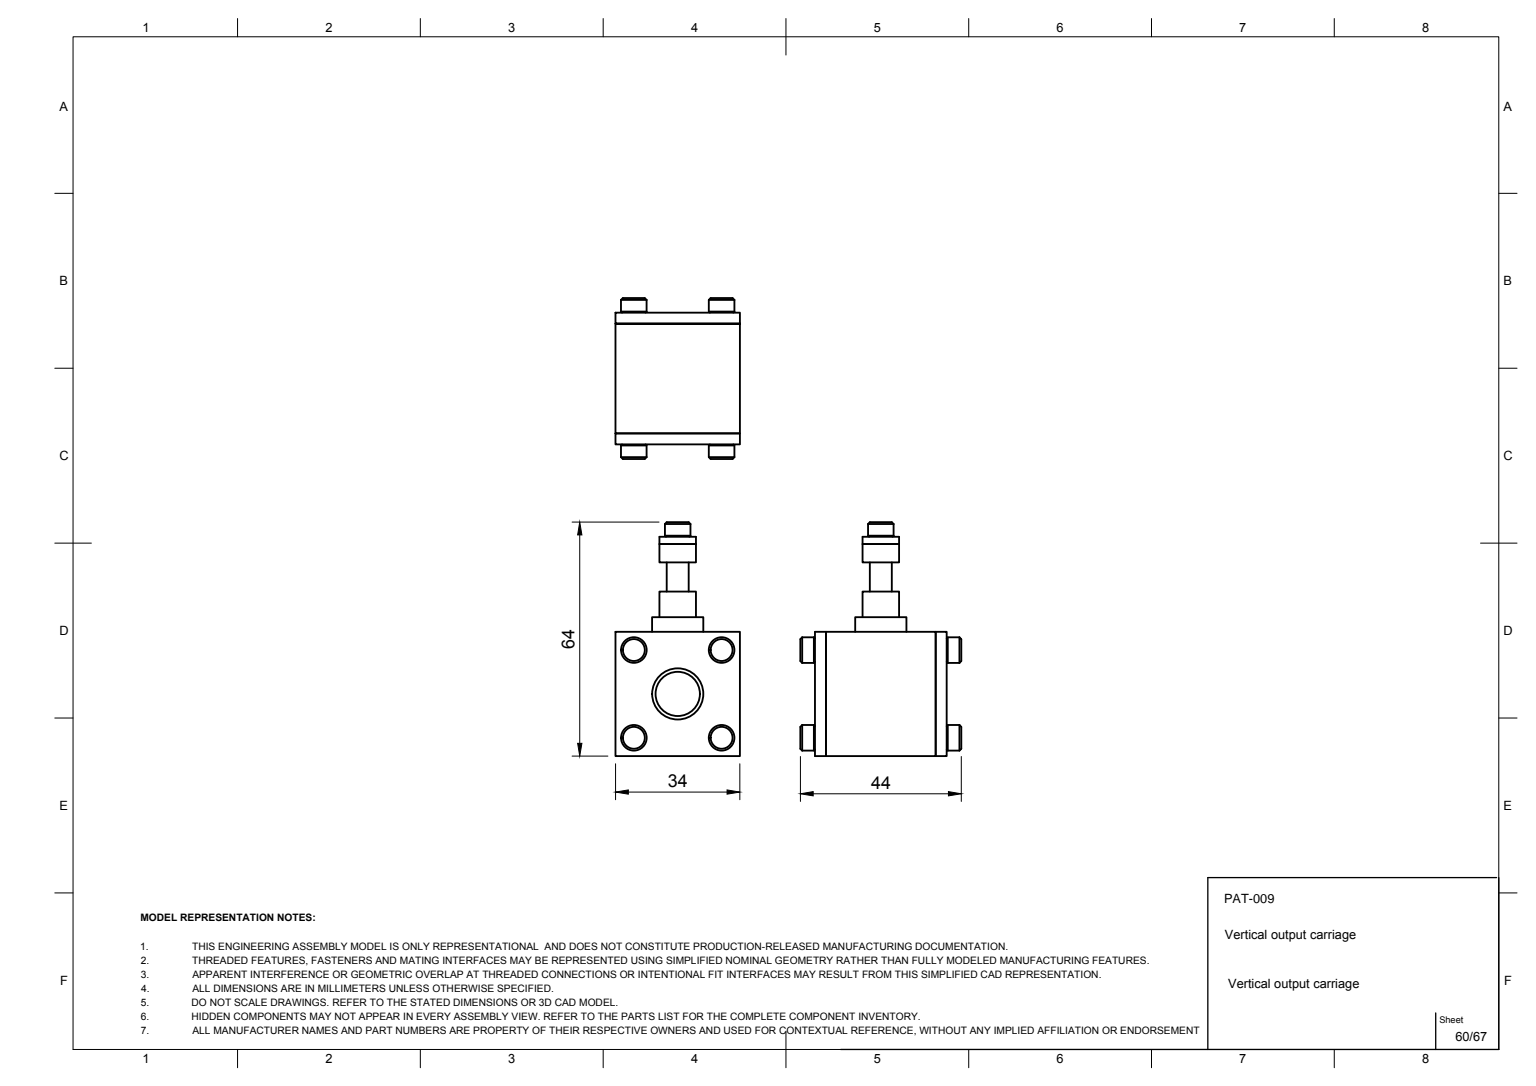
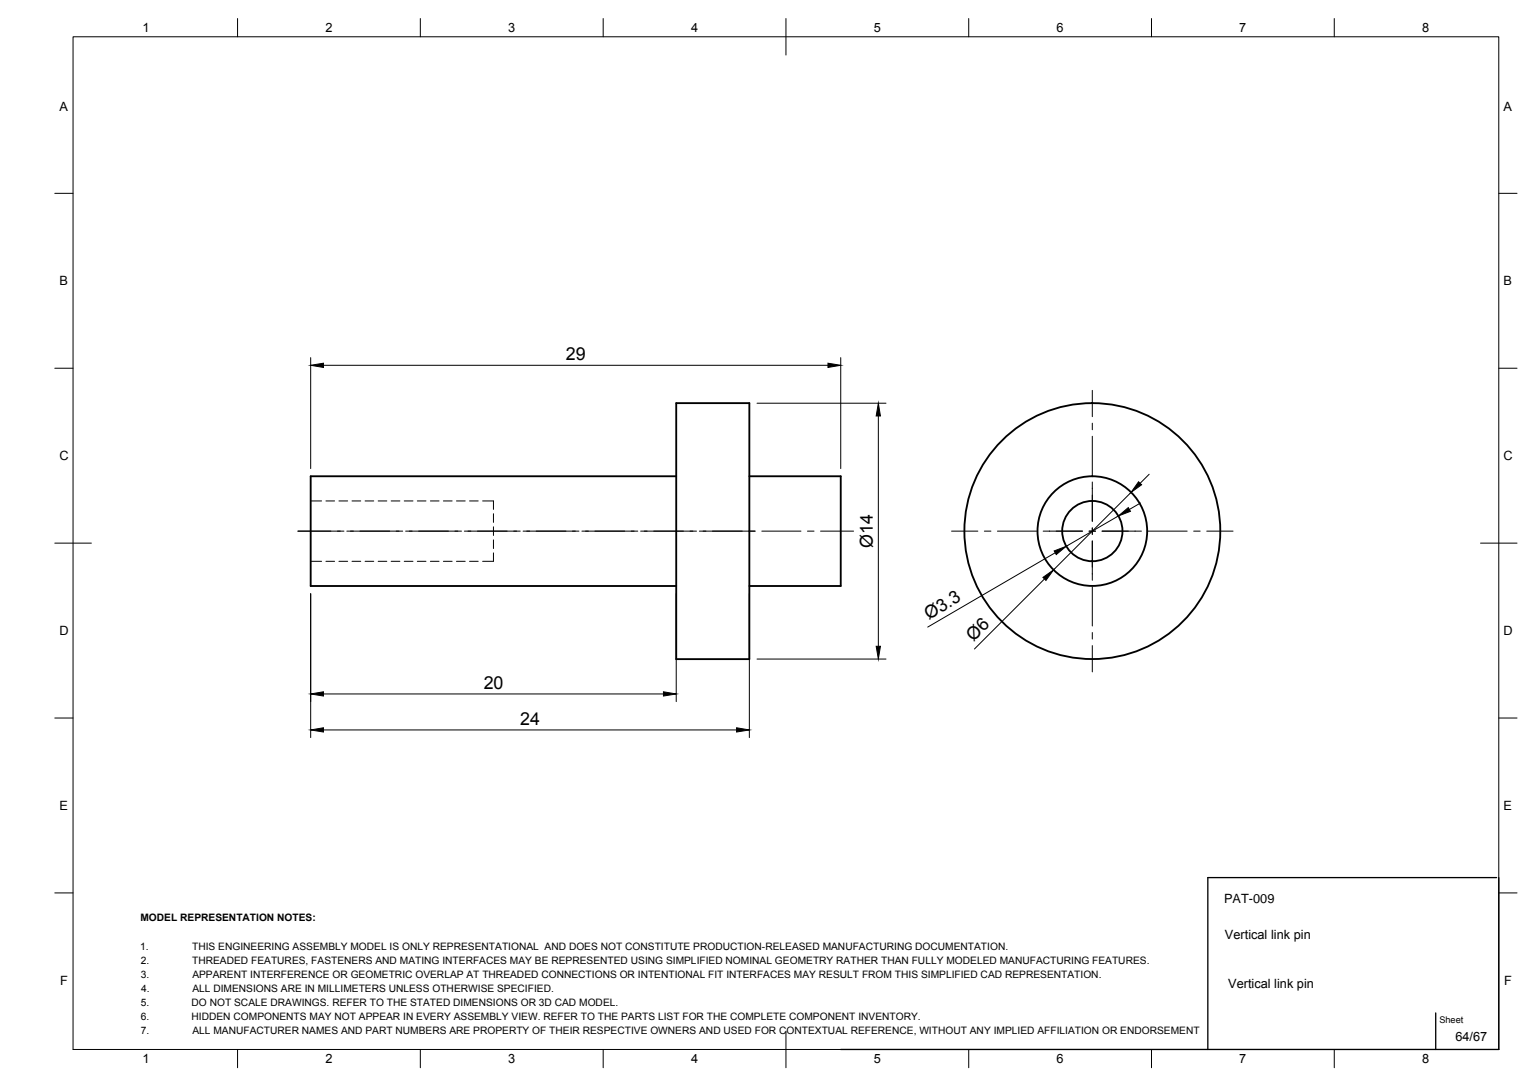
ISO-10303-21;
HEADER;
/* Generated by software containing ST-Developer
 * from STEP Tools, Inc. (www.steptools.com) 
 */

FILE_DESCRIPTION(
/* description */ ('Bell-crank linkage with push rods'),
/* implementation_level */ '2;1');

FILE_NAME(
/* name */ 'PAT-009',
/* time_stamp */ '2026-10-28T03:25:15-07:00',
/* author */ (''),
/* organization */ (''),
/* preprocessor_version */ 'ST-DEVELOPER v20.2',
/* originating_system */ 'Autodesk Translation Framework v15.17.0.0',
/* authorisation */ '');

FILE_SCHEMA (('AUTOMOTIVE_DESIGN { 1 0 10303 214 3 1 1 }'));
ENDSEC;

DATA;
#10=MECHANICAL_DESIGN_GEOMETRIC_PRESENTATION_REPRESENTATION('',(#604,#605,
#606,#607,#608,#609,#610,#611,#612,#613,#614,#615,#616,#617,#618,#619,#620,
#621,#622,#623,#624,#625,#626,#627,#628,#629,#630,#631,#632,#633,#634,#635,
#636,#637,#638,#639,#640,#641,#642,#643,#644,#645,#646,#647,#648,#649,#650,
#651,#652,#653,#654,#655,#656,#657,#658,#659,#660,#661,#662,#663,#664,#665),
#16678);
#11=ITEM_DEFINED_TRANSFORMATION($,$,#9789,#9917);
#12=ITEM_DEFINED_TRANSFORMATION($,$,#9809,#9918);
#13=ITEM_DEFINED_TRANSFORMATION($,$,#9829,#9919);
#14=ITEM_DEFINED_TRANSFORMATION($,$,#9846,#9920);
#15=ITEM_DEFINED_TRANSFORMATION($,$,#9900,#9921);
#16=ITEM_DEFINED_TRANSFORMATION($,$,#10157,#10192);
#17=ITEM_DEFINED_TRANSFORMATION($,$,#10174,#10193);
#18=ITEM_DEFINED_TRANSFORMATION($,$,#10183,#10194);
#19=ITEM_DEFINED_TRANSFORMATION($,$,#10196,#10231);
#20=ITEM_DEFINED_TRANSFORMATION($,$,#10213,#10232);
#21=ITEM_DEFINED_TRANSFORMATION($,$,#10222,#10233);
#22=ITEM_DEFINED_TRANSFORMATION($,$,#10467,#10516);
#23=ITEM_DEFINED_TRANSFORMATION($,$,#10499,#10517);
#24=ITEM_DEFINED_TRANSFORMATION($,$,#9456,#10542);
#25=ITEM_DEFINED_TRANSFORMATION($,$,#9499,#10543);
#26=ITEM_DEFINED_TRANSFORMATION($,$,#9506,#10544);
#27=ITEM_DEFINED_TRANSFORMATION($,$,#9513,#10545);
#28=ITEM_DEFINED_TRANSFORMATION($,$,#9583,#10546);
#29=ITEM_DEFINED_TRANSFORMATION($,$,#9624,#10547);
#30=ITEM_DEFINED_TRANSFORMATION($,$,#9660,#10548);
#31=ITEM_DEFINED_TRANSFORMATION($,$,#9696,#10549);
#32=ITEM_DEFINED_TRANSFORMATION($,$,#9730,#10550);
#33=ITEM_DEFINED_TRANSFORMATION($,$,#9764,#10551);
#34=ITEM_DEFINED_TRANSFORMATION($,$,#9764,#10552);
#35=ITEM_DEFINED_TRANSFORMATION($,$,#9764,#10553);
#36=ITEM_DEFINED_TRANSFORMATION($,$,#9764,#10554);
#37=ITEM_DEFINED_TRANSFORMATION($,$,#9788,#10555);
#38=ITEM_DEFINED_TRANSFORMATION($,$,#10518,#10556);
#39=ITEM_DEFINED_TRANSFORMATION($,$,#10518,#10557);
#40=ITEM_DEFINED_TRANSFORMATION($,$,#10518,#10558);
#41=ITEM_DEFINED_TRANSFORMATION($,$,#10518,#10559);
#42=ITEM_DEFINED_TRANSFORMATION($,$,#9922,#10560);
#43=ITEM_DEFINED_TRANSFORMATION($,$,#10115,#10561);
#44=ITEM_DEFINED_TRANSFORMATION($,$,#10115,#10562);
#45=ITEM_DEFINED_TRANSFORMATION($,$,#9930,#10563);
#46=ITEM_DEFINED_TRANSFORMATION($,$,#10115,#10564);
#47=ITEM_DEFINED_TRANSFORMATION($,$,#10115,#10565);
#48=ITEM_DEFINED_TRANSFORMATION($,$,#9930,#10566);
#49=ITEM_DEFINED_TRANSFORMATION($,$,#9922,#10567);
#50=ITEM_DEFINED_TRANSFORMATION($,$,#10115,#10568);
#51=ITEM_DEFINED_TRANSFORMATION($,$,#10115,#10569);
#52=ITEM_DEFINED_TRANSFORMATION($,$,#9930,#10570);
#53=ITEM_DEFINED_TRANSFORMATION($,$,#10115,#10571);
#54=ITEM_DEFINED_TRANSFORMATION($,$,#10115,#10572);
#55=ITEM_DEFINED_TRANSFORMATION($,$,#9930,#10573);
#56=ITEM_DEFINED_TRANSFORMATION($,$,#9948,#10574);
#57=ITEM_DEFINED_TRANSFORMATION($,$,#9992,#10575);
#58=ITEM_DEFINED_TRANSFORMATION($,$,#10002,#10576);
#59=ITEM_DEFINED_TRANSFORMATION($,$,#10011,#10577);
#60=ITEM_DEFINED_TRANSFORMATION($,$,#10025,#10578);
#61=ITEM_DEFINED_TRANSFORMATION($,$,#10043,#10579);
#62=ITEM_DEFINED_TRANSFORMATION($,$,#10052,#10580);
#63=ITEM_DEFINED_TRANSFORMATION($,$,#10061,#10581);
#64=ITEM_DEFINED_TRANSFORMATION($,$,#10070,#10582);
#65=ITEM_DEFINED_TRANSFORMATION($,$,#10088,#10583);
#66=ITEM_DEFINED_TRANSFORMATION($,$,#10097,#10584);
#67=ITEM_DEFINED_TRANSFORMATION($,$,#10106,#10585);
#68=ITEM_DEFINED_TRANSFORMATION($,$,#10115,#10586);
#69=ITEM_DEFINED_TRANSFORMATION($,$,#10141,#10587);
#70=ITEM_DEFINED_TRANSFORMATION($,$,#10518,#10588);
#71=ITEM_DEFINED_TRANSFORMATION($,$,#10518,#10589);
#72=ITEM_DEFINED_TRANSFORMATION($,$,#10235,#10590);
#73=ITEM_DEFINED_TRANSFORMATION($,$,#10261,#10591);
#74=ITEM_DEFINED_TRANSFORMATION($,$,#10283,#10592);
#75=ITEM_DEFINED_TRANSFORMATION($,$,#10305,#10593);
#76=ITEM_DEFINED_TRANSFORMATION($,$,#10323,#10594);
#77=ITEM_DEFINED_TRANSFORMATION($,$,#10332,#10595);
#78=ITEM_DEFINED_TRANSFORMATION($,$,#10341,#10596);
#79=ITEM_DEFINED_TRANSFORMATION($,$,#10466,#10597);
#80=ITEM_DEFINED_TRANSFORMATION($,$,#10518,#10598);
#81=ITEM_DEFINED_TRANSFORMATION($,$,#10518,#10599);
#82=ITEM_DEFINED_TRANSFORMATION($,$,#10518,#10600);
#83=ITEM_DEFINED_TRANSFORMATION($,$,#10518,#10601);
#84=ITEM_DEFINED_TRANSFORMATION($,$,#10518,#10602);
#85=ITEM_DEFINED_TRANSFORMATION($,$,#10518,#10603);
#86=ITEM_DEFINED_TRANSFORMATION($,$,#10518,#10604);
#87=ITEM_DEFINED_TRANSFORMATION($,$,#10518,#10605);
#88=ITEM_DEFINED_TRANSFORMATION($,$,#10518,#10606);
#89=ITEM_DEFINED_TRANSFORMATION($,$,#10351,#10607);
#90=ITEM_DEFINED_TRANSFORMATION($,$,#10377,#10608);
#91=ITEM_DEFINED_TRANSFORMATION($,$,#10399,#10609);
#92=ITEM_DEFINED_TRANSFORMATION($,$,#10421,#10610);
#93=ITEM_DEFINED_TRANSFORMATION($,$,#10439,#10611);
#94=ITEM_DEFINED_TRANSFORMATION($,$,#10448,#10612);
#95=ITEM_DEFINED_TRANSFORMATION($,$,#10457,#10613);
#96=ITEM_DEFINED_TRANSFORMATION($,$,#10466,#10614);
#97=ITEM_DEFINED_TRANSFORMATION($,$,#10518,#10615);
#98=ITEM_DEFINED_TRANSFORMATION($,$,#10518,#10616);
#99=ITEM_DEFINED_TRANSFORMATION($,$,#10518,#10617);
#100=ITEM_DEFINED_TRANSFORMATION($,$,#10518,#10618);
#101=ITEM_DEFINED_TRANSFORMATION($,$,#10518,#10619);
#102=ITEM_DEFINED_TRANSFORMATION($,$,#10518,#10620);
#103=ITEM_DEFINED_TRANSFORMATION($,$,#10518,#10621);
#104=ITEM_DEFINED_TRANSFORMATION($,$,#10518,#10622);
#105=ITEM_DEFINED_TRANSFORMATION($,$,#10518,#10623);
#106=ITEM_DEFINED_TRANSFORMATION($,$,#9455,#10624);
#107=ITEM_DEFINED_TRANSFORMATION($,$,#9947,#10625);
#108=ITEM_DEFINED_TRANSFORMATION($,$,#10156,#10626);
#109=ITEM_DEFINED_TRANSFORMATION($,$,#10195,#10627);
#110=ITEM_DEFINED_TRANSFORMATION($,$,#10234,#10628);
#111=ITEM_DEFINED_TRANSFORMATION($,$,#10350,#10629);
#112=(
REPRESENTATION_RELATIONSHIP($,$,#16923,#16922)
REPRESENTATION_RELATIONSHIP_WITH_TRANSFORMATION(#11)
SHAPE_REPRESENTATION_RELATIONSHIP()
);
#113=(
REPRESENTATION_RELATIONSHIP($,$,#16924,#16922)
REPRESENTATION_RELATIONSHIP_WITH_TRANSFORMATION(#12)
SHAPE_REPRESENTATION_RELATIONSHIP()
);
#114=(
REPRESENTATION_RELATIONSHIP($,$,#16925,#16922)
REPRESENTATION_RELATIONSHIP_WITH_TRANSFORMATION(#13)
SHAPE_REPRESENTATION_RELATIONSHIP()
);
#115=(
REPRESENTATION_RELATIONSHIP($,$,#16926,#16922)
REPRESENTATION_RELATIONSHIP_WITH_TRANSFORMATION(#14)
SHAPE_REPRESENTATION_RELATIONSHIP()
);
#116=(
REPRESENTATION_RELATIONSHIP($,$,#16927,#16922)
REPRESENTATION_RELATIONSHIP_WITH_TRANSFORMATION(#15)
SHAPE_REPRESENTATION_RELATIONSHIP()
);
#117=(
REPRESENTATION_RELATIONSHIP($,$,#16946,#16945)
REPRESENTATION_RELATIONSHIP_WITH_TRANSFORMATION(#16)
SHAPE_REPRESENTATION_RELATIONSHIP()
);
#118=(
REPRESENTATION_RELATIONSHIP($,$,#16947,#16945)
REPRESENTATION_RELATIONSHIP_WITH_TRANSFORMATION(#17)
SHAPE_REPRESENTATION_RELATIONSHIP()
);
#119=(
REPRESENTATION_RELATIONSHIP($,$,#16948,#16945)
REPRESENTATION_RELATIONSHIP_WITH_TRANSFORMATION(#18)
SHAPE_REPRESENTATION_RELATIONSHIP()
);
#120=(
REPRESENTATION_RELATIONSHIP($,$,#16950,#16949)
REPRESENTATION_RELATIONSHIP_WITH_TRANSFORMATION(#19)
SHAPE_REPRESENTATION_RELATIONSHIP()
);
#121=(
REPRESENTATION_RELATIONSHIP($,$,#16951,#16949)
REPRESENTATION_RELATIONSHIP_WITH_TRANSFORMATION(#20)
SHAPE_REPRESENTATION_RELATIONSHIP()
);
#122=(
REPRESENTATION_RELATIONSHIP($,$,#16952,#16949)
REPRESENTATION_RELATIONSHIP_WITH_TRANSFORMATION(#21)
SHAPE_REPRESENTATION_RELATIONSHIP()
);
#123=(
REPRESENTATION_RELATIONSHIP($,$,#16970,#16969)
REPRESENTATION_RELATIONSHIP_WITH_TRANSFORMATION(#22)
SHAPE_REPRESENTATION_RELATIONSHIP()
);
#124=(
REPRESENTATION_RELATIONSHIP($,$,#16971,#16969)
REPRESENTATION_RELATIONSHIP_WITH_TRANSFORMATION(#23)
SHAPE_REPRESENTATION_RELATIONSHIP()
);
#125=(
REPRESENTATION_RELATIONSHIP($,$,#16912,#16911)
REPRESENTATION_RELATIONSHIP_WITH_TRANSFORMATION(#24)
SHAPE_REPRESENTATION_RELATIONSHIP()
);
#126=(
REPRESENTATION_RELATIONSHIP($,$,#16913,#16911)
REPRESENTATION_RELATIONSHIP_WITH_TRANSFORMATION(#25)
SHAPE_REPRESENTATION_RELATIONSHIP()
);
#127=(
REPRESENTATION_RELATIONSHIP($,$,#16914,#16911)
REPRESENTATION_RELATIONSHIP_WITH_TRANSFORMATION(#26)
SHAPE_REPRESENTATION_RELATIONSHIP()
);
#128=(
REPRESENTATION_RELATIONSHIP($,$,#16915,#16911)
REPRESENTATION_RELATIONSHIP_WITH_TRANSFORMATION(#27)
SHAPE_REPRESENTATION_RELATIONSHIP()
);
#129=(
REPRESENTATION_RELATIONSHIP($,$,#16916,#16911)
REPRESENTATION_RELATIONSHIP_WITH_TRANSFORMATION(#28)
SHAPE_REPRESENTATION_RELATIONSHIP()
);
#130=(
REPRESENTATION_RELATIONSHIP($,$,#16917,#16911)
REPRESENTATION_RELATIONSHIP_WITH_TRANSFORMATION(#29)
SHAPE_REPRESENTATION_RELATIONSHIP()
);
#131=(
REPRESENTATION_RELATIONSHIP($,$,#16918,#16911)
REPRESENTATION_RELATIONSHIP_WITH_TRANSFORMATION(#30)
SHAPE_REPRESENTATION_RELATIONSHIP()
);
#132=(
REPRESENTATION_RELATIONSHIP($,$,#16919,#16911)
REPRESENTATION_RELATIONSHIP_WITH_TRANSFORMATION(#31)
SHAPE_REPRESENTATION_RELATIONSHIP()
);
#133=(
REPRESENTATION_RELATIONSHIP($,$,#16920,#16911)
REPRESENTATION_RELATIONSHIP_WITH_TRANSFORMATION(#32)
SHAPE_REPRESENTATION_RELATIONSHIP()
);
#134=(
REPRESENTATION_RELATIONSHIP($,$,#16921,#16911)
REPRESENTATION_RELATIONSHIP_WITH_TRANSFORMATION(#33)
SHAPE_REPRESENTATION_RELATIONSHIP()
);
#135=(
REPRESENTATION_RELATIONSHIP($,$,#16921,#16911)
REPRESENTATION_RELATIONSHIP_WITH_TRANSFORMATION(#34)
SHAPE_REPRESENTATION_RELATIONSHIP()
);
#136=(
REPRESENTATION_RELATIONSHIP($,$,#16921,#16911)
REPRESENTATION_RELATIONSHIP_WITH_TRANSFORMATION(#35)
SHAPE_REPRESENTATION_RELATIONSHIP()
);
#137=(
REPRESENTATION_RELATIONSHIP($,$,#16921,#16911)
REPRESENTATION_RELATIONSHIP_WITH_TRANSFORMATION(#36)
SHAPE_REPRESENTATION_RELATIONSHIP()
);
#138=(
REPRESENTATION_RELATIONSHIP($,$,#16922,#16911)
REPRESENTATION_RELATIONSHIP_WITH_TRANSFORMATION(#37)
SHAPE_REPRESENTATION_RELATIONSHIP()
);
#139=(
REPRESENTATION_RELATIONSHIP($,$,#16972,#16911)
REPRESENTATION_RELATIONSHIP_WITH_TRANSFORMATION(#38)
SHAPE_REPRESENTATION_RELATIONSHIP()
);
#140=(
REPRESENTATION_RELATIONSHIP($,$,#16972,#16911)
REPRESENTATION_RELATIONSHIP_WITH_TRANSFORMATION(#39)
SHAPE_REPRESENTATION_RELATIONSHIP()
);
#141=(
REPRESENTATION_RELATIONSHIP($,$,#16972,#16911)
REPRESENTATION_RELATIONSHIP_WITH_TRANSFORMATION(#40)
SHAPE_REPRESENTATION_RELATIONSHIP()
);
#142=(
REPRESENTATION_RELATIONSHIP($,$,#16972,#16911)
REPRESENTATION_RELATIONSHIP_WITH_TRANSFORMATION(#41)
SHAPE_REPRESENTATION_RELATIONSHIP()
);
#143=(
REPRESENTATION_RELATIONSHIP($,$,#16928,#16911)
REPRESENTATION_RELATIONSHIP_WITH_TRANSFORMATION(#42)
SHAPE_REPRESENTATION_RELATIONSHIP()
);
#144=(
REPRESENTATION_RELATIONSHIP($,$,#16943,#16911)
REPRESENTATION_RELATIONSHIP_WITH_TRANSFORMATION(#43)
SHAPE_REPRESENTATION_RELATIONSHIP()
);
#145=(
REPRESENTATION_RELATIONSHIP($,$,#16943,#16911)
REPRESENTATION_RELATIONSHIP_WITH_TRANSFORMATION(#44)
SHAPE_REPRESENTATION_RELATIONSHIP()
);
#146=(
REPRESENTATION_RELATIONSHIP($,$,#16929,#16911)
REPRESENTATION_RELATIONSHIP_WITH_TRANSFORMATION(#45)
SHAPE_REPRESENTATION_RELATIONSHIP()
);
#147=(
REPRESENTATION_RELATIONSHIP($,$,#16943,#16911)
REPRESENTATION_RELATIONSHIP_WITH_TRANSFORMATION(#46)
SHAPE_REPRESENTATION_RELATIONSHIP()
);
#148=(
REPRESENTATION_RELATIONSHIP($,$,#16943,#16911)
REPRESENTATION_RELATIONSHIP_WITH_TRANSFORMATION(#47)
SHAPE_REPRESENTATION_RELATIONSHIP()
);
#149=(
REPRESENTATION_RELATIONSHIP($,$,#16929,#16911)
REPRESENTATION_RELATIONSHIP_WITH_TRANSFORMATION(#48)
SHAPE_REPRESENTATION_RELATIONSHIP()
);
#150=(
REPRESENTATION_RELATIONSHIP($,$,#16928,#16911)
REPRESENTATION_RELATIONSHIP_WITH_TRANSFORMATION(#49)
SHAPE_REPRESENTATION_RELATIONSHIP()
);
#151=(
REPRESENTATION_RELATIONSHIP($,$,#16943,#16911)
REPRESENTATION_RELATIONSHIP_WITH_TRANSFORMATION(#50)
SHAPE_REPRESENTATION_RELATIONSHIP()
);
#152=(
REPRESENTATION_RELATIONSHIP($,$,#16943,#16911)
REPRESENTATION_RELATIONSHIP_WITH_TRANSFORMATION(#51)
SHAPE_REPRESENTATION_RELATIONSHIP()
);
#153=(
REPRESENTATION_RELATIONSHIP($,$,#16929,#16911)
REPRESENTATION_RELATIONSHIP_WITH_TRANSFORMATION(#52)
SHAPE_REPRESENTATION_RELATIONSHIP()
);
#154=(
REPRESENTATION_RELATIONSHIP($,$,#16943,#16911)
REPRESENTATION_RELATIONSHIP_WITH_TRANSFORMATION(#53)
SHAPE_REPRESENTATION_RELATIONSHIP()
);
#155=(
REPRESENTATION_RELATIONSHIP($,$,#16943,#16911)
REPRESENTATION_RELATIONSHIP_WITH_TRANSFORMATION(#54)
SHAPE_REPRESENTATION_RELATIONSHIP()
);
#156=(
REPRESENTATION_RELATIONSHIP($,$,#16929,#16911)
REPRESENTATION_RELATIONSHIP_WITH_TRANSFORMATION(#55)
SHAPE_REPRESENTATION_RELATIONSHIP()
);
#157=(
REPRESENTATION_RELATIONSHIP($,$,#16931,#16930)
REPRESENTATION_RELATIONSHIP_WITH_TRANSFORMATION(#56)
SHAPE_REPRESENTATION_RELATIONSHIP()
);
#158=(
REPRESENTATION_RELATIONSHIP($,$,#16932,#16930)
REPRESENTATION_RELATIONSHIP_WITH_TRANSFORMATION(#57)
SHAPE_REPRESENTATION_RELATIONSHIP()
);
#159=(
REPRESENTATION_RELATIONSHIP($,$,#16933,#16930)
REPRESENTATION_RELATIONSHIP_WITH_TRANSFORMATION(#58)
SHAPE_REPRESENTATION_RELATIONSHIP()
);
#160=(
REPRESENTATION_RELATIONSHIP($,$,#16934,#16930)
REPRESENTATION_RELATIONSHIP_WITH_TRANSFORMATION(#59)
SHAPE_REPRESENTATION_RELATIONSHIP()
);
#161=(
REPRESENTATION_RELATIONSHIP($,$,#16935,#16930)
REPRESENTATION_RELATIONSHIP_WITH_TRANSFORMATION(#60)
SHAPE_REPRESENTATION_RELATIONSHIP()
);
#162=(
REPRESENTATION_RELATIONSHIP($,$,#16936,#16930)
REPRESENTATION_RELATIONSHIP_WITH_TRANSFORMATION(#61)
SHAPE_REPRESENTATION_RELATIONSHIP()
);
#163=(
REPRESENTATION_RELATIONSHIP($,$,#16937,#16930)
REPRESENTATION_RELATIONSHIP_WITH_TRANSFORMATION(#62)
SHAPE_REPRESENTATION_RELATIONSHIP()
);
#164=(
REPRESENTATION_RELATIONSHIP($,$,#16938,#16930)
REPRESENTATION_RELATIONSHIP_WITH_TRANSFORMATION(#63)
SHAPE_REPRESENTATION_RELATIONSHIP()
);
#165=(
REPRESENTATION_RELATIONSHIP($,$,#16939,#16930)
REPRESENTATION_RELATIONSHIP_WITH_TRANSFORMATION(#64)
SHAPE_REPRESENTATION_RELATIONSHIP()
);
#166=(
REPRESENTATION_RELATIONSHIP($,$,#16940,#16930)
REPRESENTATION_RELATIONSHIP_WITH_TRANSFORMATION(#65)
SHAPE_REPRESENTATION_RELATIONSHIP()
);
#167=(
REPRESENTATION_RELATIONSHIP($,$,#16941,#16930)
REPRESENTATION_RELATIONSHIP_WITH_TRANSFORMATION(#66)
SHAPE_REPRESENTATION_RELATIONSHIP()
);
#168=(
REPRESENTATION_RELATIONSHIP($,$,#16942,#16930)
REPRESENTATION_RELATIONSHIP_WITH_TRANSFORMATION(#67)
SHAPE_REPRESENTATION_RELATIONSHIP()
);
#169=(
REPRESENTATION_RELATIONSHIP($,$,#16943,#16930)
REPRESENTATION_RELATIONSHIP_WITH_TRANSFORMATION(#68)
SHAPE_REPRESENTATION_RELATIONSHIP()
);
#170=(
REPRESENTATION_RELATIONSHIP($,$,#16944,#16930)
REPRESENTATION_RELATIONSHIP_WITH_TRANSFORMATION(#69)
SHAPE_REPRESENTATION_RELATIONSHIP()
);
#171=(
REPRESENTATION_RELATIONSHIP($,$,#16972,#16930)
REPRESENTATION_RELATIONSHIP_WITH_TRANSFORMATION(#70)
SHAPE_REPRESENTATION_RELATIONSHIP()
);
#172=(
REPRESENTATION_RELATIONSHIP($,$,#16972,#16930)
REPRESENTATION_RELATIONSHIP_WITH_TRANSFORMATION(#71)
SHAPE_REPRESENTATION_RELATIONSHIP()
);
#173=(
REPRESENTATION_RELATIONSHIP($,$,#16954,#16953)
REPRESENTATION_RELATIONSHIP_WITH_TRANSFORMATION(#72)
SHAPE_REPRESENTATION_RELATIONSHIP()
);
#174=(
REPRESENTATION_RELATIONSHIP($,$,#16955,#16953)
REPRESENTATION_RELATIONSHIP_WITH_TRANSFORMATION(#73)
SHAPE_REPRESENTATION_RELATIONSHIP()
);
#175=(
REPRESENTATION_RELATIONSHIP($,$,#16956,#16953)
REPRESENTATION_RELATIONSHIP_WITH_TRANSFORMATION(#74)
SHAPE_REPRESENTATION_RELATIONSHIP()
);
#176=(
REPRESENTATION_RELATIONSHIP($,$,#16957,#16953)
REPRESENTATION_RELATIONSHIP_WITH_TRANSFORMATION(#75)
SHAPE_REPRESENTATION_RELATIONSHIP()
);
#177=(
REPRESENTATION_RELATIONSHIP($,$,#16958,#16953)
REPRESENTATION_RELATIONSHIP_WITH_TRANSFORMATION(#76)
SHAPE_REPRESENTATION_RELATIONSHIP()
);
#178=(
REPRESENTATION_RELATIONSHIP($,$,#16959,#16953)
REPRESENTATION_RELATIONSHIP_WITH_TRANSFORMATION(#77)
SHAPE_REPRESENTATION_RELATIONSHIP()
);
#179=(
REPRESENTATION_RELATIONSHIP($,$,#16960,#16953)
REPRESENTATION_RELATIONSHIP_WITH_TRANSFORMATION(#78)
SHAPE_REPRESENTATION_RELATIONSHIP()
);
#180=(
REPRESENTATION_RELATIONSHIP($,$,#16969,#16953)
REPRESENTATION_RELATIONSHIP_WITH_TRANSFORMATION(#79)
SHAPE_REPRESENTATION_RELATIONSHIP()
);
#181=(
REPRESENTATION_RELATIONSHIP($,$,#16972,#16953)
REPRESENTATION_RELATIONSHIP_WITH_TRANSFORMATION(#80)
SHAPE_REPRESENTATION_RELATIONSHIP()
);
#182=(
REPRESENTATION_RELATIONSHIP($,$,#16972,#16953)
REPRESENTATION_RELATIONSHIP_WITH_TRANSFORMATION(#81)
SHAPE_REPRESENTATION_RELATIONSHIP()
);
#183=(
REPRESENTATION_RELATIONSHIP($,$,#16972,#16953)
REPRESENTATION_RELATIONSHIP_WITH_TRANSFORMATION(#82)
SHAPE_REPRESENTATION_RELATIONSHIP()
);
#184=(
REPRESENTATION_RELATIONSHIP($,$,#16972,#16953)
REPRESENTATION_RELATIONSHIP_WITH_TRANSFORMATION(#83)
SHAPE_REPRESENTATION_RELATIONSHIP()
);
#185=(
REPRESENTATION_RELATIONSHIP($,$,#16972,#16953)
REPRESENTATION_RELATIONSHIP_WITH_TRANSFORMATION(#84)
SHAPE_REPRESENTATION_RELATIONSHIP()
);
#186=(
REPRESENTATION_RELATIONSHIP($,$,#16972,#16953)
REPRESENTATION_RELATIONSHIP_WITH_TRANSFORMATION(#85)
SHAPE_REPRESENTATION_RELATIONSHIP()
);
#187=(
REPRESENTATION_RELATIONSHIP($,$,#16972,#16953)
REPRESENTATION_RELATIONSHIP_WITH_TRANSFORMATION(#86)
SHAPE_REPRESENTATION_RELATIONSHIP()
);
#188=(
REPRESENTATION_RELATIONSHIP($,$,#16972,#16953)
REPRESENTATION_RELATIONSHIP_WITH_TRANSFORMATION(#87)
SHAPE_REPRESENTATION_RELATIONSHIP()
);
#189=(
REPRESENTATION_RELATIONSHIP($,$,#16972,#16953)
REPRESENTATION_RELATIONSHIP_WITH_TRANSFORMATION(#88)
SHAPE_REPRESENTATION_RELATIONSHIP()
);
#190=(
REPRESENTATION_RELATIONSHIP($,$,#16962,#16961)
REPRESENTATION_RELATIONSHIP_WITH_TRANSFORMATION(#89)
SHAPE_REPRESENTATION_RELATIONSHIP()
);
#191=(
REPRESENTATION_RELATIONSHIP($,$,#16963,#16961)
REPRESENTATION_RELATIONSHIP_WITH_TRANSFORMATION(#90)
SHAPE_REPRESENTATION_RELATIONSHIP()
);
#192=(
REPRESENTATION_RELATIONSHIP($,$,#16964,#16961)
REPRESENTATION_RELATIONSHIP_WITH_TRANSFORMATION(#91)
SHAPE_REPRESENTATION_RELATIONSHIP()
);
#193=(
REPRESENTATION_RELATIONSHIP($,$,#16965,#16961)
REPRESENTATION_RELATIONSHIP_WITH_TRANSFORMATION(#92)
SHAPE_REPRESENTATION_RELATIONSHIP()
);
#194=(
REPRESENTATION_RELATIONSHIP($,$,#16966,#16961)
REPRESENTATION_RELATIONSHIP_WITH_TRANSFORMATION(#93)
SHAPE_REPRESENTATION_RELATIONSHIP()
);
#195=(
REPRESENTATION_RELATIONSHIP($,$,#16967,#16961)
REPRESENTATION_RELATIONSHIP_WITH_TRANSFORMATION(#94)
SHAPE_REPRESENTATION_RELATIONSHIP()
);
#196=(
REPRESENTATION_RELATIONSHIP($,$,#16968,#16961)
REPRESENTATION_RELATIONSHIP_WITH_TRANSFORMATION(#95)
SHAPE_REPRESENTATION_RELATIONSHIP()
);
#197=(
REPRESENTATION_RELATIONSHIP($,$,#16969,#16961)
REPRESENTATION_RELATIONSHIP_WITH_TRANSFORMATION(#96)
SHAPE_REPRESENTATION_RELATIONSHIP()
);
#198=(
REPRESENTATION_RELATIONSHIP($,$,#16972,#16961)
REPRESENTATION_RELATIONSHIP_WITH_TRANSFORMATION(#97)
SHAPE_REPRESENTATION_RELATIONSHIP()
);
#199=(
REPRESENTATION_RELATIONSHIP($,$,#16972,#16961)
REPRESENTATION_RELATIONSHIP_WITH_TRANSFORMATION(#98)
SHAPE_REPRESENTATION_RELATIONSHIP()
);
#200=(
REPRESENTATION_RELATIONSHIP($,$,#16972,#16961)
REPRESENTATION_RELATIONSHIP_WITH_TRANSFORMATION(#99)
SHAPE_REPRESENTATION_RELATIONSHIP()
);
#201=(
REPRESENTATION_RELATIONSHIP($,$,#16972,#16961)
REPRESENTATION_RELATIONSHIP_WITH_TRANSFORMATION(#100)
SHAPE_REPRESENTATION_RELATIONSHIP()
);
#202=(
REPRESENTATION_RELATIONSHIP($,$,#16972,#16961)
REPRESENTATION_RELATIONSHIP_WITH_TRANSFORMATION(#101)
SHAPE_REPRESENTATION_RELATIONSHIP()
);
#203=(
REPRESENTATION_RELATIONSHIP($,$,#16972,#16961)
REPRESENTATION_RELATIONSHIP_WITH_TRANSFORMATION(#102)
SHAPE_REPRESENTATION_RELATIONSHIP()
);
#204=(
REPRESENTATION_RELATIONSHIP($,$,#16972,#16961)
REPRESENTATION_RELATIONSHIP_WITH_TRANSFORMATION(#103)
SHAPE_REPRESENTATION_RELATIONSHIP()
);
#205=(
REPRESENTATION_RELATIONSHIP($,$,#16972,#16961)
REPRESENTATION_RELATIONSHIP_WITH_TRANSFORMATION(#104)
SHAPE_REPRESENTATION_RELATIONSHIP()
);
#206=(
REPRESENTATION_RELATIONSHIP($,$,#16972,#16961)
REPRESENTATION_RELATIONSHIP_WITH_TRANSFORMATION(#105)
SHAPE_REPRESENTATION_RELATIONSHIP()
);
#207=(
REPRESENTATION_RELATIONSHIP($,$,#16911,#16910)
REPRESENTATION_RELATIONSHIP_WITH_TRANSFORMATION(#106)
SHAPE_REPRESENTATION_RELATIONSHIP()
);
#208=(
REPRESENTATION_RELATIONSHIP($,$,#16930,#16910)
REPRESENTATION_RELATIONSHIP_WITH_TRANSFORMATION(#107)
SHAPE_REPRESENTATION_RELATIONSHIP()
);
#209=(
REPRESENTATION_RELATIONSHIP($,$,#16945,#16910)
REPRESENTATION_RELATIONSHIP_WITH_TRANSFORMATION(#108)
SHAPE_REPRESENTATION_RELATIONSHIP()
);
#210=(
REPRESENTATION_RELATIONSHIP($,$,#16949,#16910)
REPRESENTATION_RELATIONSHIP_WITH_TRANSFORMATION(#109)
SHAPE_REPRESENTATION_RELATIONSHIP()
);
#211=(
REPRESENTATION_RELATIONSHIP($,$,#16953,#16910)
REPRESENTATION_RELATIONSHIP_WITH_TRANSFORMATION(#110)
SHAPE_REPRESENTATION_RELATIONSHIP()
);
#212=(
REPRESENTATION_RELATIONSHIP($,$,#16961,#16910)
REPRESENTATION_RELATIONSHIP_WITH_TRANSFORMATION(#111)
SHAPE_REPRESENTATION_RELATIONSHIP()
);
#213=CONTEXT_DEPENDENT_SHAPE_REPRESENTATION(#112,#16764);
#214=CONTEXT_DEPENDENT_SHAPE_REPRESENTATION(#113,#16765);
#215=CONTEXT_DEPENDENT_SHAPE_REPRESENTATION(#114,#16766);
#216=CONTEXT_DEPENDENT_SHAPE_REPRESENTATION(#115,#16767);
#217=CONTEXT_DEPENDENT_SHAPE_REPRESENTATION(#116,#16768);
#218=CONTEXT_DEPENDENT_SHAPE_REPRESENTATION(#117,#16790);
#219=CONTEXT_DEPENDENT_SHAPE_REPRESENTATION(#118,#16791);
#220=CONTEXT_DEPENDENT_SHAPE_REPRESENTATION(#119,#16792);
#221=CONTEXT_DEPENDENT_SHAPE_REPRESENTATION(#120,#16797);
#222=CONTEXT_DEPENDENT_SHAPE_REPRESENTATION(#121,#16798);
#223=CONTEXT_DEPENDENT_SHAPE_REPRESENTATION(#122,#16799);
#224=CONTEXT_DEPENDENT_SHAPE_REPRESENTATION(#123,#16819);
#225=CONTEXT_DEPENDENT_SHAPE_REPRESENTATION(#124,#16820);
#226=CONTEXT_DEPENDENT_SHAPE_REPRESENTATION(#125,#16822);
#227=CONTEXT_DEPENDENT_SHAPE_REPRESENTATION(#126,#16823);
#228=CONTEXT_DEPENDENT_SHAPE_REPRESENTATION(#127,#16824);
#229=CONTEXT_DEPENDENT_SHAPE_REPRESENTATION(#128,#16825);
#230=CONTEXT_DEPENDENT_SHAPE_REPRESENTATION(#129,#16826);
#231=CONTEXT_DEPENDENT_SHAPE_REPRESENTATION(#130,#16827);
#232=CONTEXT_DEPENDENT_SHAPE_REPRESENTATION(#131,#16828);
#233=CONTEXT_DEPENDENT_SHAPE_REPRESENTATION(#132,#16829);
#234=CONTEXT_DEPENDENT_SHAPE_REPRESENTATION(#133,#16830);
#235=CONTEXT_DEPENDENT_SHAPE_REPRESENTATION(#134,#16831);
#236=CONTEXT_DEPENDENT_SHAPE_REPRESENTATION(#135,#16832);
#237=CONTEXT_DEPENDENT_SHAPE_REPRESENTATION(#136,#16833);
#238=CONTEXT_DEPENDENT_SHAPE_REPRESENTATION(#137,#16834);
#239=CONTEXT_DEPENDENT_SHAPE_REPRESENTATION(#138,#16835);
#240=CONTEXT_DEPENDENT_SHAPE_REPRESENTATION(#139,#16836);
#241=CONTEXT_DEPENDENT_SHAPE_REPRESENTATION(#140,#16837);
#242=CONTEXT_DEPENDENT_SHAPE_REPRESENTATION(#141,#16838);
#243=CONTEXT_DEPENDENT_SHAPE_REPRESENTATION(#142,#16839);
#244=CONTEXT_DEPENDENT_SHAPE_REPRESENTATION(#143,#16840);
#245=CONTEXT_DEPENDENT_SHAPE_REPRESENTATION(#144,#16841);
#246=CONTEXT_DEPENDENT_SHAPE_REPRESENTATION(#145,#16842);
#247=CONTEXT_DEPENDENT_SHAPE_REPRESENTATION(#146,#16843);
#248=CONTEXT_DEPENDENT_SHAPE_REPRESENTATION(#147,#16844);
#249=CONTEXT_DEPENDENT_SHAPE_REPRESENTATION(#148,#16845);
#250=CONTEXT_DEPENDENT_SHAPE_REPRESENTATION(#149,#16846);
#251=CONTEXT_DEPENDENT_SHAPE_REPRESENTATION(#150,#16847);
#252=CONTEXT_DEPENDENT_SHAPE_REPRESENTATION(#151,#16848);
#253=CONTEXT_DEPENDENT_SHAPE_REPRESENTATION(#152,#16849);
#254=CONTEXT_DEPENDENT_SHAPE_REPRESENTATION(#153,#16850);
#255=CONTEXT_DEPENDENT_SHAPE_REPRESENTATION(#154,#16851);
#256=CONTEXT_DEPENDENT_SHAPE_REPRESENTATION(#155,#16852);
#257=CONTEXT_DEPENDENT_SHAPE_REPRESENTATION(#156,#16853);
#258=CONTEXT_DEPENDENT_SHAPE_REPRESENTATION(#157,#16854);
#259=CONTEXT_DEPENDENT_SHAPE_REPRESENTATION(#158,#16855);
#260=CONTEXT_DEPENDENT_SHAPE_REPRESENTATION(#159,#16856);
#261=CONTEXT_DEPENDENT_SHAPE_REPRESENTATION(#160,#16857);
#262=CONTEXT_DEPENDENT_SHAPE_REPRESENTATION(#161,#16858);
#263=CONTEXT_DEPENDENT_SHAPE_REPRESENTATION(#162,#16859);
#264=CONTEXT_DEPENDENT_SHAPE_REPRESENTATION(#163,#16860);
#265=CONTEXT_DEPENDENT_SHAPE_REPRESENTATION(#164,#16861);
#266=CONTEXT_DEPENDENT_SHAPE_REPRESENTATION(#165,#16862);
#267=CONTEXT_DEPENDENT_SHAPE_REPRESENTATION(#166,#16863);
#268=CONTEXT_DEPENDENT_SHAPE_REPRESENTATION(#167,#16864);
#269=CONTEXT_DEPENDENT_SHAPE_REPRESENTATION(#168,#16865);
#270=CONTEXT_DEPENDENT_SHAPE_REPRESENTATION(#169,#16866);
#271=CONTEXT_DEPENDENT_SHAPE_REPRESENTATION(#170,#16867);
#272=CONTEXT_DEPENDENT_SHAPE_REPRESENTATION(#171,#16868);
#273=CONTEXT_DEPENDENT_SHAPE_REPRESENTATION(#172,#16869);
#274=CONTEXT_DEPENDENT_SHAPE_REPRESENTATION(#173,#16870);
#275=CONTEXT_DEPENDENT_SHAPE_REPRESENTATION(#174,#16871);
#276=CONTEXT_DEPENDENT_SHAPE_REPRESENTATION(#175,#16872);
#277=CONTEXT_DEPENDENT_SHAPE_REPRESENTATION(#176,#16873);
#278=CONTEXT_DEPENDENT_SHAPE_REPRESENTATION(#177,#16874);
#279=CONTEXT_DEPENDENT_SHAPE_REPRESENTATION(#178,#16875);
#280=CONTEXT_DEPENDENT_SHAPE_REPRESENTATION(#179,#16876);
#281=CONTEXT_DEPENDENT_SHAPE_REPRESENTATION(#180,#16877);
#282=CONTEXT_DEPENDENT_SHAPE_REPRESENTATION(#181,#16878);
#283=CONTEXT_DEPENDENT_SHAPE_REPRESENTATION(#182,#16879);
#284=CONTEXT_DEPENDENT_SHAPE_REPRESENTATION(#183,#16880);
#285=CONTEXT_DEPENDENT_SHAPE_REPRESENTATION(#184,#16881);
#286=CONTEXT_DEPENDENT_SHAPE_REPRESENTATION(#185,#16882);
#287=CONTEXT_DEPENDENT_SHAPE_REPRESENTATION(#186,#16883);
#288=CONTEXT_DEPENDENT_SHAPE_REPRESENTATION(#187,#16884);
#289=CONTEXT_DEPENDENT_SHAPE_REPRESENTATION(#188,#16885);
#290=CONTEXT_DEPENDENT_SHAPE_REPRESENTATION(#189,#16886);
#291=CONTEXT_DEPENDENT_SHAPE_REPRESENTATION(#190,#16887);
#292=CONTEXT_DEPENDENT_SHAPE_REPRESENTATION(#191,#16888);
#293=CONTEXT_DEPENDENT_SHAPE_REPRESENTATION(#192,#16889);
#294=CONTEXT_DEPENDENT_SHAPE_REPRESENTATION(#193,#16890);
#295=CONTEXT_DEPENDENT_SHAPE_REPRESENTATION(#194,#16891);
#296=CONTEXT_DEPENDENT_SHAPE_REPRESENTATION(#195,#16892);
#297=CONTEXT_DEPENDENT_SHAPE_REPRESENTATION(#196,#16893);
#298=CONTEXT_DEPENDENT_SHAPE_REPRESENTATION(#197,#16894);
#299=CONTEXT_DEPENDENT_SHAPE_REPRESENTATION(#198,#16895);
#300=CONTEXT_DEPENDENT_SHAPE_REPRESENTATION(#199,#16896);
#301=CONTEXT_DEPENDENT_SHAPE_REPRESENTATION(#200,#16897);
#302=CONTEXT_DEPENDENT_SHAPE_REPRESENTATION(#201,#16898);
#303=CONTEXT_DEPENDENT_SHAPE_REPRESENTATION(#202,#16899);
#304=CONTEXT_DEPENDENT_SHAPE_REPRESENTATION(#203,#16900);
#305=CONTEXT_DEPENDENT_SHAPE_REPRESENTATION(#204,#16901);
#306=CONTEXT_DEPENDENT_SHAPE_REPRESENTATION(#205,#16902);
#307=CONTEXT_DEPENDENT_SHAPE_REPRESENTATION(#206,#16903);
#308=CONTEXT_DEPENDENT_SHAPE_REPRESENTATION(#207,#16904);
#309=CONTEXT_DEPENDENT_SHAPE_REPRESENTATION(#208,#16905);
#310=CONTEXT_DEPENDENT_SHAPE_REPRESENTATION(#209,#16906);
#311=CONTEXT_DEPENDENT_SHAPE_REPRESENTATION(#210,#16907);
#312=CONTEXT_DEPENDENT_SHAPE_REPRESENTATION(#211,#16908);
#313=CONTEXT_DEPENDENT_SHAPE_REPRESENTATION(#212,#16909);
#314=NEXT_ASSEMBLY_USAGE_OCCURRENCE('Inner ring:1','Inner ring:1',
'Inner ring:1',#16986,#16987,'Inner ring:1');
#315=NEXT_ASSEMBLY_USAGE_OCCURRENCE('Outer ring:1','Outer ring:1',
'Outer ring:1',#16986,#16988,'Outer ring:1');
#316=NEXT_ASSEMBLY_USAGE_OCCURRENCE('Balls:1','Balls:1','Balls:1',#16986,
#16989,'Balls:1');
#317=NEXT_ASSEMBLY_USAGE_OCCURRENCE('Cage:1','Cage:1','Cage:1',#16986,#16990,
'Cage:1');
#318=NEXT_ASSEMBLY_USAGE_OCCURRENCE('Seals 2RS:1','Seals 2RS:1',
'Seals 2RS:1',#16986,#16991,'Seals 2RS:1');
#319=NEXT_ASSEMBLY_USAGE_OCCURRENCE('Horizontal connecting link:1',
'Horizontal connecting link:1','Horizontal connecting link:1',#17009,#17010,
'Horizontal connecting link:1');
#320=NEXT_ASSEMBLY_USAGE_OCCURRENCE('Plain link bushing:1',
'Plain link bushing:1','Plain link bushing:1',#17009,#17011,
'Plain link bushing:1');
#321=NEXT_ASSEMBLY_USAGE_OCCURRENCE('Plain link bushing (1):1',
'Plain link bushing (1):1','Plain link bushing (1):1',#17009,#17012,
'Plain link bushing (1):1');
#322=NEXT_ASSEMBLY_USAGE_OCCURRENCE('Vertical connecting link:1',
'Vertical connecting link:1','Vertical connecting link:1',#17013,#17014,
'Vertical connecting link:1');
#323=NEXT_ASSEMBLY_USAGE_OCCURRENCE('Plain link bushing (2):1',
'Plain link bushing (2):1','Plain link bushing (2):1',#17013,#17015,
'Plain link bushing (2):1');
#324=NEXT_ASSEMBLY_USAGE_OCCURRENCE('Plain link bushing (3):1',
'Plain link bushing (3):1','Plain link bushing (3):1',#17013,#17016,
'Plain link bushing (3):1');
#325=NEXT_ASSEMBLY_USAGE_OCCURRENCE('Steel sleeve:1','Steel sleeve:1',
'Steel sleeve:1',#17033,#17034,'Steel sleeve:1');
#326=NEXT_ASSEMBLY_USAGE_OCCURRENCE('Ball retainer (plastic):1',
'Ball retainer (plastic):1','Ball retainer (plastic):1',#17033,#17035,
'Ball retainer (plastic):1');
#327=NEXT_ASSEMBLY_USAGE_OCCURRENCE('Base:1','Base:1','Base:1',#16975,#16976,
'Base:1');
#328=NEXT_ASSEMBLY_USAGE_OCCURRENCE('Foot strip:1','Foot strip:1',
'Foot strip:1',#16975,#16977,'Foot strip:1');
#329=NEXT_ASSEMBLY_USAGE_OCCURRENCE('Foot strip (1):1',
'Foot strip (1):1','Foot strip (1):1',#16975,#16978,'Foot strip (1):1');
#330=NEXT_ASSEMBLY_USAGE_OCCURRENCE('Pivot pedestal:1',
'Pivot pedestal:1','Pivot pedestal:1',#16975,#16979,'Pivot pedestal:1');
#331=NEXT_ASSEMBLY_USAGE_OCCURRENCE('Pivot cap:1','Pivot cap:1',
'Pivot cap:1',#16975,#16980,'Pivot cap:1');
#332=NEXT_ASSEMBLY_USAGE_OCCURRENCE('Horizontal shaft support:1',
'Horizontal shaft support:1','Horizontal shaft support:1',#16975,#16981,
'Horizontal shaft support:1');
#333=NEXT_ASSEMBLY_USAGE_OCCURRENCE('Horizontal shaft support (1):1',
'Horizontal shaft support (1):1','Horizontal shaft support (1):1',#16975,
#16982,'Horizontal shaft support (1):1');
#334=NEXT_ASSEMBLY_USAGE_OCCURRENCE('Vertical shaft support:1',
'Vertical shaft support:1','Vertical shaft support:1',#16975,#16983,
'Vertical shaft support:1');
#335=NEXT_ASSEMBLY_USAGE_OCCURRENCE('Vertical shaft support (1):1',
'Vertical shaft support (1):1','Vertical shaft support (1):1',#16975,#16984,
'Vertical shaft support (1):1');
#336=NEXT_ASSEMBLY_USAGE_OCCURRENCE('M5x14 Cap Screw:2',
'M5x14 Cap Screw:2','M5x14 Cap Screw:2',#16975,#16985,
'M5x14 Cap Screw:2');
#337=NEXT_ASSEMBLY_USAGE_OCCURRENCE('M5x14 Cap Screw:3',
'M5x14 Cap Screw:3','M5x14 Cap Screw:3',#16975,#16985,
'M5x14 Cap Screw:3');
#338=NEXT_ASSEMBLY_USAGE_OCCURRENCE('M5x14 Cap Screw:4',
'M5x14 Cap Screw:4','M5x14 Cap Screw:4',#16975,#16985,
'M5x14 Cap Screw:4');
#339=NEXT_ASSEMBLY_USAGE_OCCURRENCE('M5x14 Cap Screw:5',
'M5x14 Cap Screw:5','M5x14 Cap Screw:5',#16975,#16985,
'M5x14 Cap Screw:5');
#340=NEXT_ASSEMBLY_USAGE_OCCURRENCE(
'Sealed Ball Bearing - 10 x 30 x 9 mm:2',
'Sealed Ball Bearing - 10 x 30 x 9 mm:2',
'Sealed Ball Bearing - 10 x 30 x 9 mm:2',#16975,#16986,
'Sealed Ball Bearing - 10 x 30 x 9 mm:2');
#341=NEXT_ASSEMBLY_USAGE_OCCURRENCE('M4x10 Cap Screw:2',
'M4x10 Cap Screw:2','M4x10 Cap Screw:2',#16975,#17036,
'M4x10 Cap Screw:2');
#342=NEXT_ASSEMBLY_USAGE_OCCURRENCE('M4x10 Cap Screw:3',
'M4x10 Cap Screw:3','M4x10 Cap Screw:3',#16975,#17036,
'M4x10 Cap Screw:3');
#343=NEXT_ASSEMBLY_USAGE_OCCURRENCE('M4x10 Cap Screw:4',
'M4x10 Cap Screw:4','M4x10 Cap Screw:4',#16975,#17036,
'M4x10 Cap Screw:4');
#344=NEXT_ASSEMBLY_USAGE_OCCURRENCE('M4x10 Cap Screw:5',
'M4x10 Cap Screw:5','M4x10 Cap Screw:5',#16975,#17036,
'M4x10 Cap Screw:5');
#345=NEXT_ASSEMBLY_USAGE_OCCURRENCE('Guide shaft 110 mm:2',
'Guide shaft 110 mm:2','Guide shaft 110 mm:2',#16975,#16992,
'Guide shaft 110 mm:2');
#346=NEXT_ASSEMBLY_USAGE_OCCURRENCE('Cap Screw - M4x16:3',
'Cap Screw - M4x16:3','Cap Screw - M4x16:3',#16975,#17007,
'Cap Screw - M4x16:3');
#347=NEXT_ASSEMBLY_USAGE_OCCURRENCE('Cap Screw - M4x16:4',
'Cap Screw - M4x16:4','Cap Screw - M4x16:4',#16975,#17007,
'Cap Screw - M4x16:4');
#348=NEXT_ASSEMBLY_USAGE_OCCURRENCE('Socket Set Screw - M4x6:2',
'Socket Set Screw - M4x6:2','Socket Set Screw - M4x6:2',#16975,#16993,
'Socket Set Screw - M4x6:2');
#349=NEXT_ASSEMBLY_USAGE_OCCURRENCE('Cap Screw - M4x16:5',
'Cap Screw - M4x16:5','Cap Screw - M4x16:5',#16975,#17007,
'Cap Screw - M4x16:5');
#350=NEXT_ASSEMBLY_USAGE_OCCURRENCE('Cap Screw - M4x16:6',
'Cap Screw - M4x16:6','Cap Screw - M4x16:6',#16975,#17007,
'Cap Screw - M4x16:6');
#351=NEXT_ASSEMBLY_USAGE_OCCURRENCE('Socket Set Screw - M4x6:3',
'Socket Set Screw - M4x6:3','Socket Set Screw - M4x6:3',#16975,#16993,
'Socket Set Screw - M4x6:3');
#352=NEXT_ASSEMBLY_USAGE_OCCURRENCE('Guide shaft 110 mm:3',
'Guide shaft 110 mm:3','Guide shaft 110 mm:3',#16975,#16992,
'Guide shaft 110 mm:3');
#353=NEXT_ASSEMBLY_USAGE_OCCURRENCE('Cap Screw - M4x16:7',
'Cap Screw - M4x16:7','Cap Screw - M4x16:7',#16975,#17007,
'Cap Screw - M4x16:7');
#354=NEXT_ASSEMBLY_USAGE_OCCURRENCE('Cap Screw - M4x16:8',
'Cap Screw - M4x16:8','Cap Screw - M4x16:8',#16975,#17007,
'Cap Screw - M4x16:8');
#355=NEXT_ASSEMBLY_USAGE_OCCURRENCE('Socket Set Screw - M4x6:4',
'Socket Set Screw - M4x6:4','Socket Set Screw - M4x6:4',#16975,#16993,
'Socket Set Screw - M4x6:4');
#356=NEXT_ASSEMBLY_USAGE_OCCURRENCE('Cap Screw - M4x16:9',
'Cap Screw - M4x16:9','Cap Screw - M4x16:9',#16975,#17007,
'Cap Screw - M4x16:9');
#357=NEXT_ASSEMBLY_USAGE_OCCURRENCE('Cap Screw - M4x16:10',
'Cap Screw - M4x16:10','Cap Screw - M4x16:10',#16975,#17007,
'Cap Screw - M4x16:10');
#358=NEXT_ASSEMBLY_USAGE_OCCURRENCE('Socket Set Screw - M4x6:5',
'Socket Set Screw - M4x6:5','Socket Set Screw - M4x6:5',#16975,#16993,
'Socket Set Screw - M4x6:5');
#359=NEXT_ASSEMBLY_USAGE_OCCURRENCE('Bell crank and spindle (1):1',
'Bell crank and spindle (1):1','Bell crank and spindle (1):1',#16994,#16995,
'Bell crank and spindle (1):1');
#360=NEXT_ASSEMBLY_USAGE_OCCURRENCE('Input grip:1','Input grip:1',
'Input grip:1',#16994,#16996,'Input grip:1');
#361=NEXT_ASSEMBLY_USAGE_OCCURRENCE('Lower race sleeve:1',
'Lower race sleeve:1','Lower race sleeve:1',#16994,#16997,
'Lower race sleeve:1');
#362=NEXT_ASSEMBLY_USAGE_OCCURRENCE('Spindle collar:1',
'Spindle collar:1','Spindle collar:1',#16994,#16998,'Spindle collar:1');
#363=NEXT_ASSEMBLY_USAGE_OCCURRENCE('Horizontal link pin:1',
'Horizontal link pin:1','Horizontal link pin:1',#16994,#16999,
'Horizontal link pin:1');
#364=NEXT_ASSEMBLY_USAGE_OCCURRENCE('Horizontal lower pin sleeve:1',
'Horizontal lower pin sleeve:1','Horizontal lower pin sleeve:1',#16994,
#17000,'Horizontal lower pin sleeve:1');
#365=NEXT_ASSEMBLY_USAGE_OCCURRENCE('Upper pin sleeve:1',
'Upper pin sleeve:1','Upper pin sleeve:1',#16994,#17001,
'Upper pin sleeve:1');
#366=NEXT_ASSEMBLY_USAGE_OCCURRENCE('Pin keeper:1','Pin keeper:1',
'Pin keeper:1',#16994,#17002,'Pin keeper:1');
#367=NEXT_ASSEMBLY_USAGE_OCCURRENCE('Vertical link pin:1',
'Vertical link pin:1','Vertical link pin:1',#16994,#17003,
'Vertical link pin:1');
#368=NEXT_ASSEMBLY_USAGE_OCCURRENCE('Vertical lower pin sleeve:1',
'Vertical lower pin sleeve:1','Vertical lower pin sleeve:1',#16994,#17004,
'Vertical lower pin sleeve:1');
#369=NEXT_ASSEMBLY_USAGE_OCCURRENCE('Upper pin sleeve (1):1',
'Upper pin sleeve (1):1','Upper pin sleeve (1):1',#16994,#17005,
'Upper pin sleeve (1):1');
#370=NEXT_ASSEMBLY_USAGE_OCCURRENCE('Pin keeper (1):1',
'Pin keeper (1):1','Pin keeper (1):1',#16994,#17006,'Pin keeper (1):1');
#371=NEXT_ASSEMBLY_USAGE_OCCURRENCE('Cap Screw - M4x16:2',
'Cap Screw - M4x16:2','Cap Screw - M4x16:2',#16994,#17007,
'Cap Screw - M4x16:2');
#372=NEXT_ASSEMBLY_USAGE_OCCURRENCE('M4x4 collar screw:2',
'M4x4 collar screw:2','M4x4 collar screw:2',#16994,#17008,
'M4x4 collar screw:2');
#373=NEXT_ASSEMBLY_USAGE_OCCURRENCE('M4x10 Cap Screw:14',
'M4x10 Cap Screw:14','M4x10 Cap Screw:14',#16994,#17036,
'M4x10 Cap Screw:14');
#374=NEXT_ASSEMBLY_USAGE_OCCURRENCE('M4x10 Cap Screw:24',
'M4x10 Cap Screw:24','M4x10 Cap Screw:24',#16994,#17036,
'M4x10 Cap Screw:24');
#375=NEXT_ASSEMBLY_USAGE_OCCURRENCE('Horizontal output housing:1',
'Horizontal output housing:1','Horizontal output housing:1',#17017,#17018,
'Horizontal output housing:1');
#376=NEXT_ASSEMBLY_USAGE_OCCURRENCE('Horizontal guide cap:1',
'Horizontal guide cap:1','Horizontal guide cap:1',#17017,#17019,
'Horizontal guide cap:1');
#377=NEXT_ASSEMBLY_USAGE_OCCURRENCE('Horizontal guide cap (1):1',
'Horizontal guide cap (1):1','Horizontal guide cap (1):1',#17017,#17020,
'Horizontal guide cap (1):1');
#378=NEXT_ASSEMBLY_USAGE_OCCURRENCE('Horizontal link pin (1):1',
'Horizontal link pin (1):1','Horizontal link pin (1):1',#17017,#17021,
'Horizontal link pin (1):1');
#379=NEXT_ASSEMBLY_USAGE_OCCURRENCE('Horizontal lower pin sleeve (1):1',
'Horizontal lower pin sleeve (1):1','Horizontal lower pin sleeve (1):1',
#17017,#17022,'Horizontal lower pin sleeve (1):1');
#380=NEXT_ASSEMBLY_USAGE_OCCURRENCE('Upper pin sleeve (2):1',
'Upper pin sleeve (2):1','Upper pin sleeve (2):1',#17017,#17023,
'Upper pin sleeve (2):1');
#381=NEXT_ASSEMBLY_USAGE_OCCURRENCE('Pin keeper (2):1',
'Pin keeper (2):1','Pin keeper (2):1',#17017,#17024,'Pin keeper (2):1');
#382=NEXT_ASSEMBLY_USAGE_OCCURRENCE(
'Linear Ball Bushing - 12 x 21 x 30 mm:2',
'Linear Ball Bushing - 12 x 21 x 30 mm:2',
'Linear Ball Bushing - 12 x 21 x 30 mm:2',#17017,#17033,
'Linear Ball Bushing - 12 x 21 x 30 mm:2');
#383=NEXT_ASSEMBLY_USAGE_OCCURRENCE('M4x10 Cap Screw:6',
'M4x10 Cap Screw:6','M4x10 Cap Screw:6',#17017,#17036,
'M4x10 Cap Screw:6');
#384=NEXT_ASSEMBLY_USAGE_OCCURRENCE('M4x10 Cap Screw:7',
'M4x10 Cap Screw:7','M4x10 Cap Screw:7',#17017,#17036,
'M4x10 Cap Screw:7');
#385=NEXT_ASSEMBLY_USAGE_OCCURRENCE('M4x10 Cap Screw:8',
'M4x10 Cap Screw:8','M4x10 Cap Screw:8',#17017,#17036,
'M4x10 Cap Screw:8');
#386=NEXT_ASSEMBLY_USAGE_OCCURRENCE('M4x10 Cap Screw:9',
'M4x10 Cap Screw:9','M4x10 Cap Screw:9',#17017,#17036,
'M4x10 Cap Screw:9');
#387=NEXT_ASSEMBLY_USAGE_OCCURRENCE('M4x10 Cap Screw:10',
'M4x10 Cap Screw:10','M4x10 Cap Screw:10',#17017,#17036,
'M4x10 Cap Screw:10');
#388=NEXT_ASSEMBLY_USAGE_OCCURRENCE('M4x10 Cap Screw:11',
'M4x10 Cap Screw:11','M4x10 Cap Screw:11',#17017,#17036,
'M4x10 Cap Screw:11');
#389=NEXT_ASSEMBLY_USAGE_OCCURRENCE('M4x10 Cap Screw:12',
'M4x10 Cap Screw:12','M4x10 Cap Screw:12',#17017,#17036,
'M4x10 Cap Screw:12');
#390=NEXT_ASSEMBLY_USAGE_OCCURRENCE('M4x10 Cap Screw:13',
'M4x10 Cap Screw:13','M4x10 Cap Screw:13',#17017,#17036,
'M4x10 Cap Screw:13');
#391=NEXT_ASSEMBLY_USAGE_OCCURRENCE('M4x10 Cap Screw:15',
'M4x10 Cap Screw:15','M4x10 Cap Screw:15',#17017,#17036,
'M4x10 Cap Screw:15');
#392=NEXT_ASSEMBLY_USAGE_OCCURRENCE('Vertical output housing:1',
'Vertical output housing:1','Vertical output housing:1',#17025,#17026,
'Vertical output housing:1');
#393=NEXT_ASSEMBLY_USAGE_OCCURRENCE('Vertical guide cap:1',
'Vertical guide cap:1','Vertical guide cap:1',#17025,#17027,
'Vertical guide cap:1');
#394=NEXT_ASSEMBLY_USAGE_OCCURRENCE('Vertical guide cap (1):1',
'Vertical guide cap (1):1','Vertical guide cap (1):1',#17025,#17028,
'Vertical guide cap (1):1');
#395=NEXT_ASSEMBLY_USAGE_OCCURRENCE('Vertical link pin (1):1',
'Vertical link pin (1):1','Vertical link pin (1):1',#17025,#17029,
'Vertical link pin (1):1');
#396=NEXT_ASSEMBLY_USAGE_OCCURRENCE('Vertical lower pin sleeve (1):1',
'Vertical lower pin sleeve (1):1','Vertical lower pin sleeve (1):1',#17025,
#17030,'Vertical lower pin sleeve (1):1');
#397=NEXT_ASSEMBLY_USAGE_OCCURRENCE('Upper pin sleeve (3):1',
'Upper pin sleeve (3):1','Upper pin sleeve (3):1',#17025,#17031,
'Upper pin sleeve (3):1');
#398=NEXT_ASSEMBLY_USAGE_OCCURRENCE('Pin keeper (3):1',
'Pin keeper (3):1','Pin keeper (3):1',#17025,#17032,'Pin keeper (3):1');
#399=NEXT_ASSEMBLY_USAGE_OCCURRENCE(
'Linear Ball Bushing - 12 x 21 x 30 mm:3',
'Linear Ball Bushing - 12 x 21 x 30 mm:3',
'Linear Ball Bushing - 12 x 21 x 30 mm:3',#17025,#17033,
'Linear Ball Bushing - 12 x 21 x 30 mm:3');
#400=NEXT_ASSEMBLY_USAGE_OCCURRENCE('M4x10 Cap Screw:16',
'M4x10 Cap Screw:16','M4x10 Cap Screw:16',#17025,#17036,
'M4x10 Cap Screw:16');
#401=NEXT_ASSEMBLY_USAGE_OCCURRENCE('M4x10 Cap Screw:17',
'M4x10 Cap Screw:17','M4x10 Cap Screw:17',#17025,#17036,
'M4x10 Cap Screw:17');
#402=NEXT_ASSEMBLY_USAGE_OCCURRENCE('M4x10 Cap Screw:18',
'M4x10 Cap Screw:18','M4x10 Cap Screw:18',#17025,#17036,
'M4x10 Cap Screw:18');
#403=NEXT_ASSEMBLY_USAGE_OCCURRENCE('M4x10 Cap Screw:19',
'M4x10 Cap Screw:19','M4x10 Cap Screw:19',#17025,#17036,
'M4x10 Cap Screw:19');
#404=NEXT_ASSEMBLY_USAGE_OCCURRENCE('M4x10 Cap Screw:20',
'M4x10 Cap Screw:20','M4x10 Cap Screw:20',#17025,#17036,
'M4x10 Cap Screw:20');
#405=NEXT_ASSEMBLY_USAGE_OCCURRENCE('M4x10 Cap Screw:21',
'M4x10 Cap Screw:21','M4x10 Cap Screw:21',#17025,#17036,
'M4x10 Cap Screw:21');
#406=NEXT_ASSEMBLY_USAGE_OCCURRENCE('M4x10 Cap Screw:22',
'M4x10 Cap Screw:22','M4x10 Cap Screw:22',#17025,#17036,
'M4x10 Cap Screw:22');
#407=NEXT_ASSEMBLY_USAGE_OCCURRENCE('M4x10 Cap Screw:23',
'M4x10 Cap Screw:23','M4x10 Cap Screw:23',#17025,#17036,
'M4x10 Cap Screw:23');
#408=NEXT_ASSEMBLY_USAGE_OCCURRENCE('M4x10 Cap Screw:25',
'M4x10 Cap Screw:25','M4x10 Cap Screw:25',#17025,#17036,
'M4x10 Cap Screw:25');
#409=NEXT_ASSEMBLY_USAGE_OCCURRENCE('Frame and linear guides:1',
'Frame and linear guides:1','Frame and linear guides:1',#16974,#16975,
'Frame and linear guides:1');
#410=NEXT_ASSEMBLY_USAGE_OCCURRENCE('Bell crank and spindle:1',
'Bell crank and spindle:1','Bell crank and spindle:1',#16974,#16994,
'Bell crank and spindle:1');
#411=NEXT_ASSEMBLY_USAGE_OCCURRENCE('Short-arm connecting rod:1',
'Short-arm connecting rod:1','Short-arm connecting rod:1',#16974,#17009,
'Short-arm connecting rod:1');
#412=NEXT_ASSEMBLY_USAGE_OCCURRENCE('Long-arm connecting rod:1',
'Long-arm connecting rod:1','Long-arm connecting rod:1',#16974,#17013,
'Long-arm connecting rod:1');
#413=NEXT_ASSEMBLY_USAGE_OCCURRENCE('Horizontal output carriage:1',
'Horizontal output carriage:1','Horizontal output carriage:1',#16974,#17017,
'Horizontal output carriage:1');
#414=NEXT_ASSEMBLY_USAGE_OCCURRENCE('Vertical output carriage:1',
'Vertical output carriage:1','Vertical output carriage:1',#16974,#17025,
'Vertical output carriage:1');
#415=SPHERICAL_SURFACE('',#9830,0.23815);
#416=SPHERICAL_SURFACE('',#9832,0.23815);
#417=SPHERICAL_SURFACE('',#9834,0.23815);
#418=SPHERICAL_SURFACE('',#9836,0.23815);
#419=SPHERICAL_SURFACE('',#9838,0.23815);
#420=SPHERICAL_SURFACE('',#9840,0.23815);
#421=SPHERICAL_SURFACE('',#9842,0.23815);
#422=SPHERICAL_SURFACE('',#9844,0.23815);
#423=SPHERICAL_SURFACE('',#9847,0.247676);
#424=SPHERICAL_SURFACE('',#9863,0.247676);
#425=SPHERICAL_SURFACE('',#9868,0.247676);
#426=SPHERICAL_SURFACE('',#9873,0.247676);
#427=SPHERICAL_SURFACE('',#9878,0.247676);
#428=SPHERICAL_SURFACE('',#9883,0.247676);
#429=SPHERICAL_SURFACE('',#9888,0.247676);
#430=SPHERICAL_SURFACE('',#9896,0.247676);
#431=TOROIDAL_SURFACE('',#9790,1.,0.247676);
#432=TOROIDAL_SURFACE('',#9810,1.,0.247676);
#433=CONICAL_SURFACE('',#9777,0.4,0.785398163397448);
#434=CONICAL_SURFACE('',#9781,0.41,0.785398163397448);
#435=CONICAL_SURFACE('',#9785,0.26,0.463647609000806);
#436=CONICAL_SURFACE('',#9801,0.53,0.785398163397448);
#437=CONICAL_SURFACE('',#9808,0.53,0.785398163397448);
#438=CONICAL_SURFACE('',#9821,1.47,0.785398163397449);
#439=CONICAL_SURFACE('',#9825,1.47,0.785398163397449);
#440=CONICAL_SURFACE('',#9925,0.55,0.785398163397448);
#441=CONICAL_SURFACE('',#9940,0.185,0.785398163397449);
#442=CONICAL_SURFACE('',#9944,0.1625,0.785398163397449);
#443=CONICAL_SURFACE('',#10118,0.325,0.785398163397448);
#444=CONICAL_SURFACE('',#10122,0.335,0.785398163397448);
#445=CONICAL_SURFACE('',#10126,0.21,0.463647609000806);
#446=CONICAL_SURFACE('',#10130,0.18,0.785398163397448);
#447=CONICAL_SURFACE('',#10153,0.185,0.785398163397449);
#448=CONICAL_SURFACE('',#10531,0.325,0.785398163397448);
#449=CONICAL_SURFACE('',#10535,0.335,0.785398163397448);
#450=CONICAL_SURFACE('',#10539,0.21,0.463647609000806);
#451=ORIENTED_CLOSED_SHELL('',*,#8803,.F.);
#452=ORIENTED_CLOSED_SHELL('',*,#8833,.F.);
#453=ORIENTED_CLOSED_SHELL('',*,#8857,.F.);
#454=BREP_WITH_VOIDS('Body1',#8804,(#451));
#455=BREP_WITH_VOIDS('Body1',#8832,(#452));
#456=BREP_WITH_VOIDS('Body1',#8858,(#453));
#457=B_SPLINE_CURVE_WITH_KNOTS('',3,(#13690,#13691,#13692,#13693,#13694,
#13695,#13696,#13697,#13698,#13699),.UNSPECIFIED.,.F.,.F.,(4,2,2,2,4),(0.,
0.0945941824764479,0.189188364952896,0.283770357603024,0.378352350253152),
 .UNSPECIFIED.);
#458=B_SPLINE_CURVE_WITH_KNOTS('',3,(#13700,#13701,#13702,#13703,#13704,
#13705,#13706,#13707,#13708,#13709,#13710,#13711,#13712,#13713,#13714,#13715,
#13716,#13717,#13718,#13719,#13720,#13721,#13722,#13723,#13724,#13725),
 .UNSPECIFIED.,.F.,.F.,(4,2,2,2,2,2,2,2,2,2,2,2,4),(0.378352350253152,0.47293434290328,
0.567516335553408,0.662110518029855,0.756704700506303,0.851298882982751,
0.945893065459199,1.04047505810933,1.13505705075946,1.22963904340958,1.32422103605971,
1.41881521853616,1.51340940101261),.UNSPECIFIED.);
#459=B_SPLINE_CURVE_WITH_KNOTS('',3,(#13729,#13730,#13731,#13732,#13733,
#13734,#13735,#13736,#13737,#13738,#13739,#13740,#13741,#13742,#13743,#13744,
#13745,#13746,#13747,#13748,#13749,#13750,#13751,#13752,#13753,#13754),
 .UNSPECIFIED.,.F.,.F.,(4,2,2,2,2,2,2,2,2,2,2,2,4),(0.,0.0942186410044058,
0.188437282008812,0.282655768798837,0.376874255588861,0.471092742378886,
0.565311229168911,0.659529870173317,0.753748511177723,0.847967152182129,
0.942185793186535,1.03640427997656,1.13062276676658),.UNSPECIFIED.);
#460=B_SPLINE_CURVE_WITH_KNOTS('',3,(#13755,#13756,#13757,#13758,#13759,
#13760,#13761,#13762,#13763,#13764),.UNSPECIFIED.,.F.,.F.,(4,2,2,2,4),(1.13062276676658,
1.22484125355661,1.31905974034663,1.41327838135104,1.50749702235545),
 .UNSPECIFIED.);
#461=B_SPLINE_CURVE_WITH_KNOTS('',3,(#13994,#13995,#13996,#13997,#13998,
#13999),.UNSPECIFIED.,.F.,.F.,(4,2,4),(0.635430324955934,0.687528937234029,
0.750024497760675),.UNSPECIFIED.);
#462=B_SPLINE_CURVE_WITH_KNOTS('',3,(#14003,#14004,#14005,#14006,#14007,
#14008),.UNSPECIFIED.,.F.,.F.,(4,2,4),(0.250008165920225,0.312503726446871,
0.364602338724967),.UNSPECIFIED.);
#463=B_SPLINE_CURVE_WITH_KNOTS('',3,(#14009,#14010,#14011,#14012,#14013,
#14014),.UNSPECIFIED.,.F.,.F.,(4,2,4),(0.135413993115484,0.187512605393579,
0.250008165920225),.UNSPECIFIED.);
#464=B_SPLINE_CURVE_WITH_KNOTS('',3,(#14015,#14016,#14017,#14018,#14019,
#14020),.UNSPECIFIED.,.F.,.F.,(4,2,4),(0.750024497760675,0.81252005828732,
0.864618670565416),.UNSPECIFIED.);
#465=B_SPLINE_CURVE_WITH_KNOTS('',3,(#14110,#14111,#14112,#14113,#14114,
#14115),.UNSPECIFIED.,.F.,.F.,(4,2,4),(0.635430324955932,0.687528937234027,
0.750024497760672),.UNSPECIFIED.);
#466=B_SPLINE_CURVE_WITH_KNOTS('',3,(#14119,#14120,#14121,#14122,#14123,
#14124),.UNSPECIFIED.,.F.,.F.,(4,2,4),(0.250008165920224,0.312503726446869,
0.364602338724963),.UNSPECIFIED.);
#467=B_SPLINE_CURVE_WITH_KNOTS('',3,(#14125,#14126,#14127,#14128,#14129,
#14130),.UNSPECIFIED.,.F.,.F.,(4,2,4),(0.135413993115483,0.187512605393579,
0.250008165920224),.UNSPECIFIED.);
#468=B_SPLINE_CURVE_WITH_KNOTS('',3,(#14131,#14132,#14133,#14134,#14135,
#14136),.UNSPECIFIED.,.F.,.F.,(4,2,4),(0.750024497760672,0.812520058287317,
0.864618670565412),.UNSPECIFIED.);
#469=B_SPLINE_CURVE_WITH_KNOTS('',3,(#14216,#14217,#14218,#14219,#14220,
#14221,#14222,#14223,#14224,#14225),.UNSPECIFIED.,.F.,.F.,(4,2,2,2,4),(0.635430324955937,
0.687528937234029,0.750024497760675,0.81252005828732,0.864618670565412),
 .UNSPECIFIED.);
#470=B_SPLINE_CURVE_WITH_KNOTS('',3,(#14233,#14234,#14235,#14236,#14237,
#14238,#14239,#14240,#14241,#14242),.UNSPECIFIED.,.F.,.F.,(4,2,2,2,4),(0.135413993115487,
0.187512605393579,0.250008165920225,0.312503726446871,0.364602338724964),
 .UNSPECIFIED.);
#471=B_SPLINE_CURVE_WITH_KNOTS('',3,(#14321,#14322,#14323,#14324,#14325,
#14326,#14327,#14328,#14329,#14330),.UNSPECIFIED.,.F.,.F.,(4,2,2,2,4),(0.635430324955933,
0.687528937234029,0.750024497760674,0.81252005828732,0.86461867056541),
 .UNSPECIFIED.);
#472=B_SPLINE_CURVE_WITH_KNOTS('',3,(#14338,#14339,#14340,#14341,#14342,
#14343,#14344,#14345,#14346,#14347),.UNSPECIFIED.,.F.,.F.,(4,2,2,2,4),(0.135413993115484,
0.187512605393579,0.250008165920225,0.31250372644687,0.364602338724967),
 .UNSPECIFIED.);
#473=B_SPLINE_CURVE_WITH_KNOTS('',3,(#14583,#14584,#14585,#14586,#14587,
#14588,#14589,#14590,#14591,#14592,#14593,#14594,#14595,#14596,#14597,#14598,
#14599,#14600,#14601,#14602,#14603,#14604),.UNSPECIFIED.,.F.,.F.,(4,2,2,
2,2,2,2,2,2,2,4),(0.0473477652366656,0.126350602536658,0.189525903804987,
0.252701205073317,0.313298422430275,0.373895639787233,0.434492857144191,
0.495090074501149,0.558265375769478,0.621440677037807,0.7004435143378),
 .UNSPECIFIED.);
#474=B_SPLINE_CURVE_WITH_KNOTS('',3,(#14608,#14609,#14610,#14611,#14612,
#14613,#14614,#14615,#14616,#14617,#14618,#14619,#14620,#14621,#14622,#14623,
#14624,#14625,#14626,#14627,#14628,#14629),.UNSPECIFIED.,.F.,.F.,(4,2,2,
2,2,2,2,2,2,2,4),(0.0464897534940957,0.0852567806515119,0.170513561303024,
0.246687263103517,0.308657850341199,0.370628437578881,0.432599024816563,
0.494569612054245,0.570743313854739,0.656000094506251,0.694767121663666),
 .UNSPECIFIED.);
#475=B_SPLINE_CURVE_WITH_KNOTS('',3,(#14635,#14636,#14637,#14638,#14639,
#14640,#14641,#14642,#14643,#14644,#14645,#14646,#14647,#14648,#14649,#14650,
#14651,#14652,#14653,#14654,#14655,#14656),.UNSPECIFIED.,.F.,.F.,(4,2,2,
2,2,2,2,2,2,2,4),(0.0464897534940957,0.0852567806515118,0.170513561303024,
0.246687263103517,0.308657850341199,0.370628437578881,0.432599024816563,
0.494569612054245,0.570743313854738,0.65600009450625,0.694767121663666),
 .UNSPECIFIED.);
#476=B_SPLINE_CURVE_WITH_KNOTS('',3,(#14660,#14661,#14662,#14663,#14664,
#14665,#14666,#14667,#14668,#14669,#14670,#14671,#14672,#14673,#14674,#14675,
#14676,#14677,#14678,#14679,#14680,#14681),.UNSPECIFIED.,.F.,.F.,(4,2,2,
2,2,2,2,2,2,2,4),(0.0464897534940957,0.0852567806515119,0.170513561303024,
0.246687263103517,0.308657850341199,0.370628437578881,0.432599024816563,
0.494569612054245,0.570743313854739,0.656000094506251,0.694767121663666),
 .UNSPECIFIED.);
#477=B_SPLINE_CURVE_WITH_KNOTS('',3,(#14685,#14686,#14687,#14688,#14689,
#14690,#14691,#14692,#14693,#14694,#14695,#14696),.UNSPECIFIED.,.F.,.F.,
(4,2,2,2,2,4),(0.0464897534940957,0.0852567806515119,0.170513561303024,
0.246687263103517,0.308657850341199,0.370628437578881),.UNSPECIFIED.);
#478=B_SPLINE_CURVE_WITH_KNOTS('',3,(#14701,#14702,#14703,#14704,#14705,
#14706,#14707,#14708,#14709,#14710,#14711,#14712),.UNSPECIFIED.,.F.,.F.,
(4,2,2,2,2,4),(0.370628437578881,0.432599024816563,0.494569612054245,0.570743313854738,
0.65600009450625,0.694767121663666),.UNSPECIFIED.);
#479=B_SPLINE_CURVE_WITH_KNOTS('',3,(#14716,#14717,#14718,#14719,#14720,
#14721,#14722,#14723,#14724,#14725,#14726,#14727,#14728,#14729,#14730,#14731,
#14732,#14733,#14734,#14735,#14736,#14737),.UNSPECIFIED.,.F.,.F.,(4,2,2,
2,2,2,2,2,2,2,4),(0.0464897534940957,0.0852567806515121,0.170513561303024,
0.246687263103518,0.308657850341199,0.370628437578881,0.432599024816563,
0.494569612054245,0.570743313854738,0.65600009450625,0.694767121663666),
 .UNSPECIFIED.);
#480=B_SPLINE_CURVE_WITH_KNOTS('',3,(#14741,#14742,#14743,#14744,#14745,
#14746,#14747,#14748,#14749,#14750,#14751,#14752,#14753,#14754,#14755,#14756,
#14757,#14758,#14759,#14760,#14761,#14762),.UNSPECIFIED.,.F.,.F.,(4,2,2,
2,2,2,2,2,2,2,4),(0.0464897534940957,0.0852567806515119,0.170513561303024,
0.246687263103517,0.308657850341199,0.370628437578881,0.432599024816563,
0.494569612054245,0.570743313854738,0.65600009450625,0.694767121663667),
 .UNSPECIFIED.);
#481=B_SPLINE_CURVE_WITH_KNOTS('',3,(#14766,#14767,#14768,#14769,#14770,
#14771,#14772,#14773,#14774,#14775,#14776,#14777,#14778,#14779,#14780,#14781,
#14782,#14783,#14784,#14785,#14786,#14787),.UNSPECIFIED.,.F.,.F.,(4,2,2,
2,2,2,2,2,2,2,4),(0.0464897534940957,0.0852567806515119,0.170513561303024,
0.246687263103517,0.308657850341199,0.370628437578881,0.432599024816563,
0.494569612054245,0.570743313854738,0.65600009450625,0.694767121663666),
 .UNSPECIFIED.);
#482=B_SPLINE_CURVE_WITH_KNOTS('',3,(#14791,#14792,#14793,#14794,#14795,
#14796,#14797,#14798,#14799,#14800,#14801,#14802,#14803,#14804,#14805,#14806,
#14807,#14808,#14809,#14810,#14811,#14812),.UNSPECIFIED.,.F.,.F.,(4,2,2,
2,2,2,2,2,2,2,4),(0.0464897534940957,0.0852567806515119,0.170513561303024,
0.246687263103517,0.308657850341199,0.370628437578881,0.432599024816563,
0.494569612054245,0.570743313854739,0.656000094506251,0.694767121663667),
 .UNSPECIFIED.);
#483=B_SPLINE_CURVE_WITH_KNOTS('',3,(#14820,#14821,#14822,#14823,#14824,
#14825,#14826,#14827,#14828,#14829,#14830,#14831,#14832,#14833,#14834,#14835,
#14836,#14837,#14838,#14839,#14840,#14841),.UNSPECIFIED.,.F.,.F.,(4,2,2,
2,2,2,2,2,2,2,4),(0.0473477652366656,0.126350602536658,0.189525903804987,
0.252701205073316,0.313298422430274,0.373895639787232,0.434492857144191,
0.495090074501149,0.558265375769478,0.621440677037807,0.7004435143378),
 .UNSPECIFIED.);
#484=B_SPLINE_CURVE_WITH_KNOTS('',3,(#14849,#14850,#14851,#14852,#14853,
#14854,#14855,#14856,#14857,#14858,#14859,#14860,#14861,#14862,#14863,#14864,
#14865,#14866,#14867,#14868,#14869,#14870),.UNSPECIFIED.,.F.,.F.,(4,2,2,
2,2,2,2,2,2,2,4),(0.0473477652366656,0.126350602536658,0.189525903804987,
0.252701205073317,0.313298422430275,0.373895639787233,0.434492857144191,
0.495090074501149,0.558265375769478,0.621440677037807,0.7004435143378),
 .UNSPECIFIED.);
#485=B_SPLINE_CURVE_WITH_KNOTS('',3,(#14879,#14880,#14881,#14882,#14883,
#14884,#14885,#14886,#14887,#14888,#14889,#14890),.UNSPECIFIED.,.F.,.F.,
(4,2,2,2,2,4),(0.0473477652366656,0.126350602536658,0.189525903804987,0.252701205073316,
0.313298422430275,0.373895639787233),.UNSPECIFIED.);
#486=B_SPLINE_CURVE_WITH_KNOTS('',3,(#14892,#14893,#14894,#14895,#14896,
#14897,#14898,#14899,#14900,#14901,#14902,#14903),.UNSPECIFIED.,.F.,.F.,
(4,2,2,2,2,4),(0.373895639787233,0.434492857144191,0.495090074501149,0.558265375769478,
0.621440677037807,0.7004435143378),.UNSPECIFIED.);
#487=B_SPLINE_CURVE_WITH_KNOTS('',3,(#14910,#14911,#14912,#14913,#14914,
#14915,#14916,#14917,#14918,#14919,#14920,#14921,#14922,#14923,#14924,#14925,
#14926,#14927,#14928,#14929,#14930,#14931),.UNSPECIFIED.,.F.,.F.,(4,2,2,
2,2,2,2,2,2,2,4),(0.0473477652366656,0.126350602536658,0.189525903804987,
0.252701205073316,0.313298422430275,0.373895639787233,0.434492857144191,
0.495090074501149,0.558265375769478,0.621440677037807,0.7004435143378),
 .UNSPECIFIED.);
#488=B_SPLINE_CURVE_WITH_KNOTS('',3,(#14939,#14940,#14941,#14942,#14943,
#14944,#14945,#14946,#14947,#14948,#14949,#14950,#14951,#14952,#14953,#14954,
#14955,#14956,#14957,#14958,#14959,#14960),.UNSPECIFIED.,.F.,.F.,(4,2,2,
2,2,2,2,2,2,2,4),(0.0473477652366656,0.126350602536658,0.189525903804987,
0.252701205073317,0.313298422430275,0.373895639787233,0.434492857144191,
0.495090074501149,0.558265375769478,0.621440677037807,0.7004435143378),
 .UNSPECIFIED.);
#489=B_SPLINE_CURVE_WITH_KNOTS('',3,(#14968,#14969,#14970,#14971,#14972,
#14973,#14974,#14975,#14976,#14977,#14978,#14979,#14980,#14981,#14982,#14983,
#14984,#14985,#14986,#14987,#14988,#14989),.UNSPECIFIED.,.F.,.F.,(4,2,2,
2,2,2,2,2,2,2,4),(0.0473477652366656,0.126350602536658,0.189525903804987,
0.252701205073316,0.313298422430275,0.373895639787233,0.434492857144191,
0.495090074501149,0.558265375769478,0.621440677037807,0.7004435143378),
 .UNSPECIFIED.);
#490=B_SPLINE_CURVE_WITH_KNOTS('',3,(#14998,#14999,#15000,#15001,#15002,
#15003,#15004,#15005,#15006,#15007,#15008,#15009,#15010,#15011,#15012,#15013,
#15014,#15015,#15016,#15017,#15018,#15019),.UNSPECIFIED.,.F.,.F.,(4,2,2,
2,2,2,2,2,2,2,4),(0.0473477652366656,0.126350602536658,0.189525903804987,
0.252701205073317,0.313298422430275,0.373895639787233,0.434492857144191,
0.495090074501149,0.558265375769478,0.621440677037807,0.7004435143378),
 .UNSPECIFIED.);
#491=B_SPLINE_CURVE_WITH_KNOTS('',3,(#15275,#15276,#15277,#15278,#15279,
#15280,#15281,#15282,#15283,#15284,#15285,#15286,#15287,#15288),
 .UNSPECIFIED.,.F.,.F.,(4,2,2,2,2,2,4),(0.618551524396293,0.626563103102765,
0.689203386094988,0.751843669087211,0.814483952079434,0.877124235071657,
0.88513581377813),.UNSPECIFIED.);
#492=B_SPLINE_CURVE_WITH_KNOTS('',3,(#15292,#15293,#15294,#15295,#15296,
#15297,#15298,#15299),.UNSPECIFIED.,.F.,.F.,(4,2,2,4),(0.250614556362404,
0.313254839354627,0.37589512234685,0.383906701053323),.UNSPECIFIED.);
#493=B_SPLINE_CURVE_WITH_KNOTS('',3,(#15303,#15304,#15305,#15306,#15307,
#15308,#15309,#15310,#15311,#15312,#15313,#15314,#15315,#15316,#15317,#15318,
#15319,#15320,#15321,#15322,#15323,#15324,#15325,#15326,#15327,#15328),
 .UNSPECIFIED.,.F.,.F.,(4,2,2,2,2,2,2,2,2,2,2,2,4),(0.,0.0623062782223143,
0.124612556444629,0.186916384615149,0.249220212785669,0.31152404095619,
0.37382786912671,0.436134147349024,0.498440425571339,0.560746703793653,
0.623052982015967,0.685356810186488,0.747660638357008),.UNSPECIFIED.);
#494=B_SPLINE_CURVE_WITH_KNOTS('',3,(#15329,#15330,#15331,#15332,#15333,
#15334,#15335,#15336,#15337,#15338),.UNSPECIFIED.,.F.,.F.,(4,2,2,2,4),(0.747660638357008,
0.809964466527528,0.872268294698049,0.934574572920363,0.996880851142677),
 .UNSPECIFIED.);
#495=B_SPLINE_CURVE_WITH_KNOTS('',3,(#15339,#15340,#15341,#15342,#15343,
#15344,#15345,#15346),.UNSPECIFIED.,.F.,.F.,(4,2,2,4),(0.117322411671485,
0.125333990377958,0.187974273370181,0.250614556362404),.UNSPECIFIED.);
#496=SHAPE_REPRESENTATION_RELATIONSHIP('SRR','None',#16912,#550);
#497=SHAPE_REPRESENTATION_RELATIONSHIP('SRR','None',#16913,#551);
#498=SHAPE_REPRESENTATION_RELATIONSHIP('SRR','None',#16914,#552);
#499=SHAPE_REPRESENTATION_RELATIONSHIP('SRR','None',#16915,#553);
#500=SHAPE_REPRESENTATION_RELATIONSHIP('SRR','None',#16916,#554);
#501=SHAPE_REPRESENTATION_RELATIONSHIP('SRR','None',#16917,#555);
#502=SHAPE_REPRESENTATION_RELATIONSHIP('SRR','None',#16918,#556);
#503=SHAPE_REPRESENTATION_RELATIONSHIP('SRR','None',#16919,#557);
#504=SHAPE_REPRESENTATION_RELATIONSHIP('SRR','None',#16920,#558);
#505=SHAPE_REPRESENTATION_RELATIONSHIP('SRR','None',#16921,#559);
#506=SHAPE_REPRESENTATION_RELATIONSHIP('SRR','None',#16923,#560);
#507=SHAPE_REPRESENTATION_RELATIONSHIP('SRR','None',#16924,#561);
#508=SHAPE_REPRESENTATION_RELATIONSHIP('SRR','None',#16925,#562);
#509=SHAPE_REPRESENTATION_RELATIONSHIP('SRR','None',#16926,#563);
#510=SHAPE_REPRESENTATION_RELATIONSHIP('SRR','None',#16927,#564);
#511=SHAPE_REPRESENTATION_RELATIONSHIP('SRR','None',#16928,#565);
#512=SHAPE_REPRESENTATION_RELATIONSHIP('SRR','None',#16929,#566);
#513=SHAPE_REPRESENTATION_RELATIONSHIP('SRR','None',#16931,#567);
#514=SHAPE_REPRESENTATION_RELATIONSHIP('SRR','None',#16932,#568);
#515=SHAPE_REPRESENTATION_RELATIONSHIP('SRR','None',#16933,#569);
#516=SHAPE_REPRESENTATION_RELATIONSHIP('SRR','None',#16934,#570);
#517=SHAPE_REPRESENTATION_RELATIONSHIP('SRR','None',#16935,#571);
#518=SHAPE_REPRESENTATION_RELATIONSHIP('SRR','None',#16936,#572);
#519=SHAPE_REPRESENTATION_RELATIONSHIP('SRR','None',#16937,#573);
#520=SHAPE_REPRESENTATION_RELATIONSHIP('SRR','None',#16938,#574);
#521=SHAPE_REPRESENTATION_RELATIONSHIP('SRR','None',#16939,#575);
#522=SHAPE_REPRESENTATION_RELATIONSHIP('SRR','None',#16940,#576);
#523=SHAPE_REPRESENTATION_RELATIONSHIP('SRR','None',#16941,#577);
#524=SHAPE_REPRESENTATION_RELATIONSHIP('SRR','None',#16942,#578);
#525=SHAPE_REPRESENTATION_RELATIONSHIP('SRR','None',#16943,#579);
#526=SHAPE_REPRESENTATION_RELATIONSHIP('SRR','None',#16944,#580);
#527=SHAPE_REPRESENTATION_RELATIONSHIP('SRR','None',#16946,#581);
#528=SHAPE_REPRESENTATION_RELATIONSHIP('SRR','None',#16947,#582);
#529=SHAPE_REPRESENTATION_RELATIONSHIP('SRR','None',#16948,#583);
#530=SHAPE_REPRESENTATION_RELATIONSHIP('SRR','None',#16950,#584);
#531=SHAPE_REPRESENTATION_RELATIONSHIP('SRR','None',#16951,#585);
#532=SHAPE_REPRESENTATION_RELATIONSHIP('SRR','None',#16952,#586);
#533=SHAPE_REPRESENTATION_RELATIONSHIP('SRR','None',#16954,#587);
#534=SHAPE_REPRESENTATION_RELATIONSHIP('SRR','None',#16955,#588);
#535=SHAPE_REPRESENTATION_RELATIONSHIP('SRR','None',#16956,#589);
#536=SHAPE_REPRESENTATION_RELATIONSHIP('SRR','None',#16957,#590);
#537=SHAPE_REPRESENTATION_RELATIONSHIP('SRR','None',#16958,#591);
#538=SHAPE_REPRESENTATION_RELATIONSHIP('SRR','None',#16959,#592);
#539=SHAPE_REPRESENTATION_RELATIONSHIP('SRR','None',#16960,#593);
#540=SHAPE_REPRESENTATION_RELATIONSHIP('SRR','None',#16962,#594);
#541=SHAPE_REPRESENTATION_RELATIONSHIP('SRR','None',#16963,#595);
#542=SHAPE_REPRESENTATION_RELATIONSHIP('SRR','None',#16964,#596);
#543=SHAPE_REPRESENTATION_RELATIONSHIP('SRR','None',#16965,#597);
#544=SHAPE_REPRESENTATION_RELATIONSHIP('SRR','None',#16966,#598);
#545=SHAPE_REPRESENTATION_RELATIONSHIP('SRR','None',#16967,#599);
#546=SHAPE_REPRESENTATION_RELATIONSHIP('SRR','None',#16968,#600);
#547=SHAPE_REPRESENTATION_RELATIONSHIP('SRR','None',#16970,#601);
#548=SHAPE_REPRESENTATION_RELATIONSHIP('SRR','None',#16971,#602);
#549=SHAPE_REPRESENTATION_RELATIONSHIP('SRR','None',#16972,#603);
#550=ADVANCED_BREP_SHAPE_REPRESENTATION('',(#666),#16617);
#551=ADVANCED_BREP_SHAPE_REPRESENTATION('',(#667),#16618);
#552=ADVANCED_BREP_SHAPE_REPRESENTATION('',(#668),#16619);
#553=ADVANCED_BREP_SHAPE_REPRESENTATION('',(#669),#16620);
#554=ADVANCED_BREP_SHAPE_REPRESENTATION('',(#670),#16621);
#555=ADVANCED_BREP_SHAPE_REPRESENTATION('',(#671),#16622);
#556=ADVANCED_BREP_SHAPE_REPRESENTATION('',(#672),#16623);
#557=ADVANCED_BREP_SHAPE_REPRESENTATION('',(#673),#16624);
#558=ADVANCED_BREP_SHAPE_REPRESENTATION('',(#674),#16625);
#559=ADVANCED_BREP_SHAPE_REPRESENTATION('',(#454),#16626);
#560=ADVANCED_BREP_SHAPE_REPRESENTATION('',(#675),#16628);
#561=ADVANCED_BREP_SHAPE_REPRESENTATION('',(#676),#16629);
#562=ADVANCED_BREP_SHAPE_REPRESENTATION('',(#677,#678,#679,#680,#681,#682,
#683,#684),#16630);
#563=ADVANCED_BREP_SHAPE_REPRESENTATION('',(#685),#16631);
#564=ADVANCED_BREP_SHAPE_REPRESENTATION('',(#686,#687),#16632);
#565=ADVANCED_BREP_SHAPE_REPRESENTATION('',(#688),#16633);
#566=ADVANCED_BREP_SHAPE_REPRESENTATION('',(#689),#16634);
#567=ADVANCED_BREP_SHAPE_REPRESENTATION('',(#690),#16636);
#568=ADVANCED_BREP_SHAPE_REPRESENTATION('',(#691),#16637);
#569=ADVANCED_BREP_SHAPE_REPRESENTATION('',(#692),#16638);
#570=ADVANCED_BREP_SHAPE_REPRESENTATION('',(#693),#16639);
#571=ADVANCED_BREP_SHAPE_REPRESENTATION('',(#694),#16640);
#572=ADVANCED_BREP_SHAPE_REPRESENTATION('',(#695),#16641);
#573=ADVANCED_BREP_SHAPE_REPRESENTATION('',(#696),#16642);
#574=ADVANCED_BREP_SHAPE_REPRESENTATION('',(#697),#16643);
#575=ADVANCED_BREP_SHAPE_REPRESENTATION('',(#698),#16644);
#576=ADVANCED_BREP_SHAPE_REPRESENTATION('',(#699),#16645);
#577=ADVANCED_BREP_SHAPE_REPRESENTATION('',(#700),#16646);
#578=ADVANCED_BREP_SHAPE_REPRESENTATION('',(#701),#16647);
#579=ADVANCED_BREP_SHAPE_REPRESENTATION('',(#455),#16648);
#580=ADVANCED_BREP_SHAPE_REPRESENTATION('',(#702),#16649);
#581=ADVANCED_BREP_SHAPE_REPRESENTATION('',(#703),#16651);
#582=ADVANCED_BREP_SHAPE_REPRESENTATION('',(#704),#16652);
#583=ADVANCED_BREP_SHAPE_REPRESENTATION('',(#705),#16653);
#584=ADVANCED_BREP_SHAPE_REPRESENTATION('',(#706),#16655);
#585=ADVANCED_BREP_SHAPE_REPRESENTATION('',(#707),#16656);
#586=ADVANCED_BREP_SHAPE_REPRESENTATION('',(#708),#16657);
#587=ADVANCED_BREP_SHAPE_REPRESENTATION('',(#709),#16659);
#588=ADVANCED_BREP_SHAPE_REPRESENTATION('',(#710),#16660);
#589=ADVANCED_BREP_SHAPE_REPRESENTATION('',(#711),#16661);
#590=ADVANCED_BREP_SHAPE_REPRESENTATION('',(#712),#16662);
#591=ADVANCED_BREP_SHAPE_REPRESENTATION('',(#713),#16663);
#592=ADVANCED_BREP_SHAPE_REPRESENTATION('',(#714),#16664);
#593=ADVANCED_BREP_SHAPE_REPRESENTATION('',(#715),#16665);
#594=ADVANCED_BREP_SHAPE_REPRESENTATION('',(#716),#16667);
#595=ADVANCED_BREP_SHAPE_REPRESENTATION('',(#717),#16668);
#596=ADVANCED_BREP_SHAPE_REPRESENTATION('',(#718),#16669);
#597=ADVANCED_BREP_SHAPE_REPRESENTATION('',(#719),#16670);
#598=ADVANCED_BREP_SHAPE_REPRESENTATION('',(#720),#16671);
#599=ADVANCED_BREP_SHAPE_REPRESENTATION('',(#721),#16672);
#600=ADVANCED_BREP_SHAPE_REPRESENTATION('',(#722),#16673);
#601=ADVANCED_BREP_SHAPE_REPRESENTATION('',(#723),#16675);
#602=ADVANCED_BREP_SHAPE_REPRESENTATION('',(#724),#16676);
#603=ADVANCED_BREP_SHAPE_REPRESENTATION('',(#456),#16677);
#604=STYLED_ITEM('',(#17270),#666);
#605=STYLED_ITEM('',(#17277),#667);
#606=STYLED_ITEM('',(#17277),#668);
#607=STYLED_ITEM('',(#17305),#669);
#608=STYLED_ITEM('',(#17277),#670);
#609=STYLED_ITEM('',(#17291),#671);
#610=STYLED_ITEM('',(#17291),#672);
#611=STYLED_ITEM('',(#17291),#673);
#612=STYLED_ITEM('',(#17291),#674);
#613=STYLED_ITEM('',(#17298),#454);
#614=STYLED_ITEM('',(#17291),#675);
#615=STYLED_ITEM('',(#17291),#676);
#616=STYLED_ITEM('',(#17291),#677);
#617=STYLED_ITEM('',(#17291),#678);
#618=STYLED_ITEM('',(#17291),#679);
#619=STYLED_ITEM('',(#17291),#680);
#620=STYLED_ITEM('',(#17291),#681);
#621=STYLED_ITEM('',(#17291),#682);
#622=STYLED_ITEM('',(#17291),#683);
#623=STYLED_ITEM('',(#17291),#684);
#624=STYLED_ITEM('',(#17291),#685);
#625=STYLED_ITEM('',(#17291),#686);
#626=STYLED_ITEM('',(#17291),#687);
#627=STYLED_ITEM('',(#17291),#688);
#628=STYLED_ITEM('',(#17298),#689);
#629=STYLED_ITEM('',(#17284),#690);
#630=STYLED_ITEM('',(#17298),#691);
#631=STYLED_ITEM('',(#17277),#692);
#632=STYLED_ITEM('',(#17284),#693);
#633=STYLED_ITEM('',(#17291),#694);
#634=STYLED_ITEM('',(#17291),#695);
#635=STYLED_ITEM('',(#17291),#696);
#636=STYLED_ITEM('',(#17291),#697);
#637=STYLED_ITEM('',(#17291),#698);
#638=STYLED_ITEM('',(#17291),#699);
#639=STYLED_ITEM('',(#17291),#700);
#640=STYLED_ITEM('',(#17291),#701);
#641=STYLED_ITEM('',(#17298),#455);
#642=STYLED_ITEM('',(#17298),#702);
#643=STYLED_ITEM('',(#17277),#703);
#644=STYLED_ITEM('',(#17284),#704);
#645=STYLED_ITEM('',(#17284),#705);
#646=STYLED_ITEM('',(#17277),#706);
#647=STYLED_ITEM('',(#17284),#707);
#648=STYLED_ITEM('',(#17284),#708);
#649=STYLED_ITEM('',(#17270),#709);
#650=STYLED_ITEM('',(#17284),#710);
#651=STYLED_ITEM('',(#17284),#711);
#652=STYLED_ITEM('',(#17291),#712);
#653=STYLED_ITEM('',(#17291),#713);
#654=STYLED_ITEM('',(#17291),#714);
#655=STYLED_ITEM('',(#17291),#715);
#656=STYLED_ITEM('',(#17270),#716);
#657=STYLED_ITEM('',(#17277),#717);
#658=STYLED_ITEM('',(#17277),#718);
#659=STYLED_ITEM('',(#17291),#719);
#660=STYLED_ITEM('',(#17291),#720);
#661=STYLED_ITEM('',(#17291),#721);
#662=STYLED_ITEM('',(#17291),#722);
#663=STYLED_ITEM('',(#17305),#723);
#664=STYLED_ITEM('',(#17284),#724);
#665=STYLED_ITEM('',(#17298),#456);
#666=MANIFOLD_SOLID_BREP('Body1',#8794);
#667=MANIFOLD_SOLID_BREP('Body1',#8795);
#668=MANIFOLD_SOLID_BREP('Body1',#8796);
#669=MANIFOLD_SOLID_BREP('Body1',#8797);
#670=MANIFOLD_SOLID_BREP('Body1',#8798);
#671=MANIFOLD_SOLID_BREP('Body1',#8799);
#672=MANIFOLD_SOLID_BREP('Body1',#8800);
#673=MANIFOLD_SOLID_BREP('Body1',#8801);
#674=MANIFOLD_SOLID_BREP('Body1',#8802);
#675=MANIFOLD_SOLID_BREP('Body1',#8805);
#676=MANIFOLD_SOLID_BREP('Body1',#8806);
#677=MANIFOLD_SOLID_BREP('Body1',#8807);
#678=MANIFOLD_SOLID_BREP('Body2',#8808);
#679=MANIFOLD_SOLID_BREP('Body3',#8809);
#680=MANIFOLD_SOLID_BREP('Body4',#8810);
#681=MANIFOLD_SOLID_BREP('Body5',#8811);
#682=MANIFOLD_SOLID_BREP('Body6',#8812);
#683=MANIFOLD_SOLID_BREP('Body7',#8813);
#684=MANIFOLD_SOLID_BREP('Body8',#8814);
#685=MANIFOLD_SOLID_BREP('Continuous crown cage',#8815);
#686=MANIFOLD_SOLID_BREP('Body1',#8816);
#687=MANIFOLD_SOLID_BREP('Body2',#8817);
#688=MANIFOLD_SOLID_BREP('Body1',#8818);
#689=MANIFOLD_SOLID_BREP('Body1',#8819);
#690=MANIFOLD_SOLID_BREP('Body1',#8820);
#691=MANIFOLD_SOLID_BREP('Body1',#8821);
#692=MANIFOLD_SOLID_BREP('Body1',#8822);
#693=MANIFOLD_SOLID_BREP('Body1',#8823);
#694=MANIFOLD_SOLID_BREP('Body1',#8824);
#695=MANIFOLD_SOLID_BREP('Body1',#8825);
#696=MANIFOLD_SOLID_BREP('Body1',#8826);
#697=MANIFOLD_SOLID_BREP('Body1',#8827);
#698=MANIFOLD_SOLID_BREP('Body1',#8828);
#699=MANIFOLD_SOLID_BREP('Body1',#8829);
#700=MANIFOLD_SOLID_BREP('Body1',#8830);
#701=MANIFOLD_SOLID_BREP('Body1',#8831);
#702=MANIFOLD_SOLID_BREP('Body1',#8834);
#703=MANIFOLD_SOLID_BREP('Body1',#8835);
#704=MANIFOLD_SOLID_BREP('Body1',#8836);
#705=MANIFOLD_SOLID_BREP('Body1',#8837);
#706=MANIFOLD_SOLID_BREP('Body1',#8838);
#707=MANIFOLD_SOLID_BREP('Body1',#8839);
#708=MANIFOLD_SOLID_BREP('Body1',#8840);
#709=MANIFOLD_SOLID_BREP('Body1',#8841);
#710=MANIFOLD_SOLID_BREP('Body1',#8842);
#711=MANIFOLD_SOLID_BREP('Body1',#8843);
#712=MANIFOLD_SOLID_BREP('Body1',#8844);
#713=MANIFOLD_SOLID_BREP('Body1',#8845);
#714=MANIFOLD_SOLID_BREP('Body1',#8846);
#715=MANIFOLD_SOLID_BREP('Body1',#8847);
#716=MANIFOLD_SOLID_BREP('Body1',#8848);
#717=MANIFOLD_SOLID_BREP('Body1',#8849);
#718=MANIFOLD_SOLID_BREP('Body1',#8850);
#719=MANIFOLD_SOLID_BREP('Body1',#8851);
#720=MANIFOLD_SOLID_BREP('Body1',#8852);
#721=MANIFOLD_SOLID_BREP('Body1',#8853);
#722=MANIFOLD_SOLID_BREP('Body1',#8854);
#723=MANIFOLD_SOLID_BREP('Body1',#8855);
#724=MANIFOLD_SOLID_BREP('Body1',#8856);
#725=FACE_BOUND('',#1786,.T.);
#726=FACE_BOUND('',#1787,.T.);
#727=FACE_BOUND('',#1788,.T.);
#728=FACE_BOUND('',#1789,.T.);
#729=FACE_BOUND('',#1790,.T.);
#730=FACE_BOUND('',#1791,.T.);
#731=FACE_BOUND('',#1792,.T.);
#732=FACE_BOUND('',#1793,.T.);
#733=FACE_BOUND('',#1794,.T.);
#734=FACE_BOUND('',#1795,.T.);
#735=FACE_BOUND('',#1796,.T.);
#736=FACE_BOUND('',#1797,.T.);
#737=FACE_BOUND('',#1799,.T.);
#738=FACE_BOUND('',#1800,.T.);
#739=FACE_BOUND('',#1801,.T.);
#740=FACE_BOUND('',#1802,.T.);
#741=FACE_BOUND('',#1803,.T.);
#742=FACE_BOUND('',#1804,.T.);
#743=FACE_BOUND('',#1805,.T.);
#744=FACE_BOUND('',#1806,.T.);
#745=FACE_BOUND('',#1807,.T.);
#746=FACE_BOUND('',#1808,.T.);
#747=FACE_BOUND('',#1809,.T.);
#748=FACE_BOUND('',#1810,.T.);
#749=FACE_BOUND('',#1842,.T.);
#750=FACE_BOUND('',#1843,.T.);
#751=FACE_BOUND('',#1844,.T.);
#752=FACE_BOUND('',#1845,.T.);
#753=FACE_BOUND('',#1846,.T.);
#754=FACE_BOUND('',#1853,.T.);
#755=FACE_BOUND('',#1855,.T.);
#756=FACE_BOUND('',#1857,.T.);
#757=FACE_BOUND('',#1859,.T.);
#758=FACE_BOUND('',#1860,.T.);
#759=FACE_BOUND('',#1861,.T.);
#760=FACE_BOUND('',#1862,.T.);
#761=FACE_BOUND('',#1863,.T.);
#762=FACE_BOUND('',#1865,.T.);
#763=FACE_BOUND('',#1866,.T.);
#764=FACE_BOUND('',#1867,.T.);
#765=FACE_BOUND('',#1868,.T.);
#766=FACE_BOUND('',#1869,.T.);
#767=FACE_BOUND('',#1872,.T.);
#768=FACE_BOUND('',#1875,.T.);
#769=FACE_BOUND('',#1878,.T.);
#770=FACE_BOUND('',#1881,.T.);
#771=FACE_BOUND('',#1888,.T.);
#772=FACE_BOUND('',#1892,.T.);
#773=FACE_BOUND('',#1893,.T.);
#774=FACE_BOUND('',#1894,.T.);
#775=FACE_BOUND('',#1895,.T.);
#776=FACE_BOUND('',#1896,.T.);
#777=FACE_BOUND('',#1898,.T.);
#778=FACE_BOUND('',#1899,.T.);
#779=FACE_BOUND('',#1900,.T.);
#780=FACE_BOUND('',#1901,.T.);
#781=FACE_BOUND('',#1902,.T.);
#782=FACE_BOUND('',#1910,.T.);
#783=FACE_BOUND('',#1913,.T.);
#784=FACE_BOUND('',#1915,.T.);
#785=FACE_BOUND('',#1921,.T.);
#786=FACE_BOUND('',#1924,.T.);
#787=FACE_BOUND('',#1926,.T.);
#788=FACE_BOUND('',#1927,.T.);
#789=FACE_BOUND('',#1935,.T.);
#790=FACE_BOUND('',#1938,.T.);
#791=FACE_BOUND('',#1940,.T.);
#792=FACE_BOUND('',#1946,.T.);
#793=FACE_BOUND('',#1949,.T.);
#794=FACE_BOUND('',#1951,.T.);
#795=FACE_BOUND('',#1952,.T.);
#796=FACE_BOUND('',#1959,.T.);
#797=FACE_BOUND('',#1962,.T.);
#798=FACE_BOUND('',#1964,.T.);
#799=FACE_BOUND('',#1968,.T.);
#800=FACE_BOUND('',#1970,.T.);
#801=FACE_BOUND('',#1973,.T.);
#802=FACE_BOUND('',#1976,.T.);
#803=FACE_BOUND('',#1977,.T.);
#804=FACE_BOUND('',#1984,.T.);
#805=FACE_BOUND('',#1987,.T.);
#806=FACE_BOUND('',#1989,.T.);
#807=FACE_BOUND('',#1993,.T.);
#808=FACE_BOUND('',#1995,.T.);
#809=FACE_BOUND('',#1998,.T.);
#810=FACE_BOUND('',#2001,.T.);
#811=FACE_BOUND('',#2002,.T.);
#812=FACE_BOUND('',#2017,.T.);
#813=FACE_BOUND('',#2025,.T.);
#814=FACE_BOUND('',#2028,.T.);
#815=FACE_BOUND('',#2033,.T.);
#816=FACE_BOUND('',#2038,.T.);
#817=FACE_BOUND('',#2066,.T.);
#818=FACE_BOUND('',#2069,.T.);
#819=FACE_BOUND('',#2072,.T.);
#820=FACE_BOUND('',#2075,.T.);
#821=FACE_BOUND('',#2078,.T.);
#822=FACE_BOUND('',#2092,.T.);
#823=FACE_BOUND('',#2103,.T.);
#824=FACE_BOUND('',#2104,.T.);
#825=FACE_BOUND('',#2105,.T.);
#826=FACE_BOUND('',#2112,.T.);
#827=FACE_BOUND('',#2113,.T.);
#828=FACE_BOUND('',#2114,.T.);
#829=FACE_BOUND('',#2115,.T.);
#830=FACE_BOUND('',#2122,.T.);
#831=FACE_BOUND('',#2131,.T.);
#832=FACE_BOUND('',#2135,.T.);
#833=FACE_BOUND('',#2137,.T.);
#834=FACE_BOUND('',#2142,.T.);
#835=FACE_BOUND('',#2144,.T.);
#836=FACE_BOUND('',#2146,.T.);
#837=FACE_BOUND('',#2148,.T.);
#838=FACE_BOUND('',#2152,.T.);
#839=FACE_BOUND('',#2154,.T.);
#840=FACE_BOUND('',#2159,.T.);
#841=FACE_BOUND('',#2164,.T.);
#842=FACE_BOUND('',#2166,.T.);
#843=FACE_BOUND('',#2170,.T.);
#844=FACE_BOUND('',#2172,.T.);
#845=FACE_BOUND('',#2176,.T.);
#846=FACE_BOUND('',#2178,.T.);
#847=FACE_BOUND('',#2182,.T.);
#848=FACE_BOUND('',#2184,.T.);
#849=FACE_BOUND('',#2189,.T.);
#850=FACE_BOUND('',#2194,.T.);
#851=FACE_BOUND('',#2196,.T.);
#852=FACE_BOUND('',#2200,.T.);
#853=FACE_BOUND('',#2202,.T.);
#854=FACE_BOUND('',#2206,.T.);
#855=FACE_BOUND('',#2208,.T.);
#856=FACE_BOUND('',#2214,.T.);
#857=FACE_BOUND('',#2236,.T.);
#858=FACE_BOUND('',#2244,.T.);
#859=FACE_BOUND('',#2245,.T.);
#860=FACE_BOUND('',#2249,.T.);
#861=FACE_BOUND('',#2250,.T.);
#862=FACE_BOUND('',#2254,.T.);
#863=FACE_BOUND('',#2256,.T.);
#864=FACE_BOUND('',#2260,.T.);
#865=FACE_BOUND('',#2262,.T.);
#866=FACE_BOUND('',#2268,.T.);
#867=FACE_BOUND('',#2269,.T.);
#868=FACE_BOUND('',#2273,.T.);
#869=FACE_BOUND('',#2274,.T.);
#870=FACE_BOUND('',#2278,.T.);
#871=FACE_BOUND('',#2280,.T.);
#872=FACE_BOUND('',#2284,.T.);
#873=FACE_BOUND('',#2286,.T.);
#874=FACE_BOUND('',#2296,.T.);
#875=FACE_BOUND('',#2297,.T.);
#876=FACE_BOUND('',#2298,.T.);
#877=FACE_BOUND('',#2299,.T.);
#878=FACE_BOUND('',#2300,.T.);
#879=FACE_BOUND('',#2303,.T.);
#880=FACE_BOUND('',#2304,.T.);
#881=FACE_BOUND('',#2305,.T.);
#882=FACE_BOUND('',#2306,.T.);
#883=FACE_BOUND('',#2307,.T.);
#884=FACE_BOUND('',#2309,.T.);
#885=FACE_BOUND('',#2318,.T.);
#886=FACE_BOUND('',#2319,.T.);
#887=FACE_BOUND('',#2320,.T.);
#888=FACE_BOUND('',#2321,.T.);
#889=FACE_BOUND('',#2322,.T.);
#890=FACE_BOUND('',#2325,.T.);
#891=FACE_BOUND('',#2326,.T.);
#892=FACE_BOUND('',#2327,.T.);
#893=FACE_BOUND('',#2328,.T.);
#894=FACE_BOUND('',#2329,.T.);
#895=FACE_BOUND('',#2339,.T.);
#896=FACE_BOUND('',#2340,.T.);
#897=FACE_BOUND('',#2341,.T.);
#898=FACE_BOUND('',#2342,.T.);
#899=FACE_BOUND('',#2343,.T.);
#900=FACE_BOUND('',#2346,.T.);
#901=FACE_BOUND('',#2347,.T.);
#902=FACE_BOUND('',#2348,.T.);
#903=FACE_BOUND('',#2349,.T.);
#904=FACE_BOUND('',#2350,.T.);
#905=FACE_BOUND('',#2356,.T.);
#906=FACE_BOUND('',#2358,.T.);
#907=FACE_BOUND('',#2363,.T.);
#908=FACE_BOUND('',#2368,.T.);
#909=FACE_BOUND('',#2370,.T.);
#910=FACE_BOUND('',#2374,.T.);
#911=FACE_BOUND('',#2376,.T.);
#912=FACE_BOUND('',#2380,.T.);
#913=FACE_BOUND('',#2382,.T.);
#914=FACE_BOUND('',#2391,.T.);
#915=FACE_BOUND('',#2392,.T.);
#916=FACE_BOUND('',#2393,.T.);
#917=FACE_BOUND('',#2394,.T.);
#918=FACE_BOUND('',#2395,.T.);
#919=FACE_BOUND('',#2398,.T.);
#920=FACE_BOUND('',#2399,.T.);
#921=FACE_BOUND('',#2400,.T.);
#922=FACE_BOUND('',#2401,.T.);
#923=FACE_BOUND('',#2402,.T.);
#924=FACE_BOUND('',#2405,.T.);
#925=FACE_BOUND('',#2413,.T.);
#926=FACE_BOUND('',#2414,.T.);
#927=FACE_BOUND('',#2415,.T.);
#928=FACE_BOUND('',#2416,.T.);
#929=FACE_BOUND('',#2417,.T.);
#930=FACE_BOUND('',#2420,.T.);
#931=FACE_BOUND('',#2421,.T.);
#932=FACE_BOUND('',#2422,.T.);
#933=FACE_BOUND('',#2423,.T.);
#934=FACE_BOUND('',#2424,.T.);
#935=FACE_BOUND('',#2434,.T.);
#936=FACE_BOUND('',#2435,.T.);
#937=FACE_BOUND('',#2436,.T.);
#938=FACE_BOUND('',#2437,.T.);
#939=FACE_BOUND('',#2438,.T.);
#940=FACE_BOUND('',#2441,.T.);
#941=FACE_BOUND('',#2442,.T.);
#942=FACE_BOUND('',#2443,.T.);
#943=FACE_BOUND('',#2444,.T.);
#944=FACE_BOUND('',#2445,.T.);
#945=FACE_BOUND('',#2452,.T.);
#946=FACE_BOUND('',#2454,.T.);
#947=FACE_BOUND('',#2459,.T.);
#948=FACE_BOUND('',#2464,.T.);
#949=FACE_BOUND('',#2466,.T.);
#950=FACE_BOUND('',#2470,.T.);
#951=FACE_BOUND('',#2472,.T.);
#952=FACE_BOUND('',#2476,.T.);
#953=FACE_BOUND('',#2478,.T.);
#954=FACE_BOUND('',#2485,.T.);
#955=FACE_BOUND('',#2488,.T.);
#956=FACE_BOUND('',#2491,.T.);
#957=FACE_BOUND('',#2494,.T.);
#958=FACE_BOUND('',#2497,.T.);
#959=FACE_BOUND('',#2500,.T.);
#960=FACE_BOUND('',#2502,.T.);
#961=FACE_BOUND('',#2508,.T.);
#962=FACE_BOUND('',#2510,.T.);
#963=FACE_BOUND('',#2512,.T.);
#964=FACE_BOUND('',#2514,.T.);
#965=FACE_BOUND('',#2529,.T.);
#966=PLANE('',#9493);
#967=PLANE('',#9494);
#968=PLANE('',#9495);
#969=PLANE('',#9496);
#970=PLANE('',#9497);
#971=PLANE('',#9498);
#972=PLANE('',#9500);
#973=PLANE('',#9501);
#974=PLANE('',#9502);
#975=PLANE('',#9503);
#976=PLANE('',#9504);
#977=PLANE('',#9505);
#978=PLANE('',#9507);
#979=PLANE('',#9508);
#980=PLANE('',#9509);
#981=PLANE('',#9510);
#982=PLANE('',#9511);
#983=PLANE('',#9512);
#984=PLANE('',#9518);
#985=PLANE('',#9522);
#986=PLANE('',#9526);
#987=PLANE('',#9530);
#988=PLANE('',#9531);
#989=PLANE('',#9539);
#990=PLANE('',#9544);
#991=PLANE('',#9549);
#992=PLANE('',#9558);
#993=PLANE('',#9575);
#994=PLANE('',#9581);
#995=PLANE('',#9582);
#996=PLANE('',#9587);
#997=PLANE('',#9592);
#998=PLANE('',#9597);
#999=PLANE('',#9602);
#1000=PLANE('',#9615);
#1001=PLANE('',#9622);
#1002=PLANE('',#9623);
#1003=PLANE('',#9631);
#1004=PLANE('',#9636);
#1005=PLANE('',#9640);
#1006=PLANE('',#9645);
#1007=PLANE('',#9647);
#1008=PLANE('',#9655);
#1009=PLANE('',#9656);
#1010=PLANE('',#9657);
#1011=PLANE('',#9658);
#1012=PLANE('',#9659);
#1013=PLANE('',#9667);
#1014=PLANE('',#9672);
#1015=PLANE('',#9676);
#1016=PLANE('',#9681);
#1017=PLANE('',#9683);
#1018=PLANE('',#9691);
#1019=PLANE('',#9692);
#1020=PLANE('',#9693);
#1021=PLANE('',#9694);
#1022=PLANE('',#9695);
#1023=PLANE('',#9700);
#1024=PLANE('',#9706);
#1025=PLANE('',#9710);
#1026=PLANE('',#9715);
#1027=PLANE('',#9717);
#1028=PLANE('',#9725);
#1029=PLANE('',#9726);
#1030=PLANE('',#9727);
#1031=PLANE('',#9728);
#1032=PLANE('',#9729);
#1033=PLANE('',#9734);
#1034=PLANE('',#9740);
#1035=PLANE('',#9744);
#1036=PLANE('',#9749);
#1037=PLANE('',#9751);
#1038=PLANE('',#9759);
#1039=PLANE('',#9760);
#1040=PLANE('',#9761);
#1041=PLANE('',#9762);
#1042=PLANE('',#9763);
#1043=PLANE('',#9765);
#1044=PLANE('',#9766);
#1045=PLANE('',#9767);
#1046=PLANE('',#9768);
#1047=PLANE('',#9769);
#1048=PLANE('',#9770);
#1049=PLANE('',#9771);
#1050=PLANE('',#9772);
#1051=PLANE('',#9773);
#1052=PLANE('',#9775);
#1053=PLANE('',#9783);
#1054=PLANE('',#9803);
#1055=PLANE('',#9806);
#1056=PLANE('',#9818);
#1057=PLANE('',#9827);
#1058=PLANE('',#9860);
#1059=PLANE('',#9865);
#1060=PLANE('',#9870);
#1061=PLANE('',#9875);
#1062=PLANE('',#9880);
#1063=PLANE('',#9885);
#1064=PLANE('',#9894);
#1065=PLANE('',#9898);
#1066=PLANE('',#9899);
#1067=PLANE('',#9901);
#1068=PLANE('',#9906);
#1069=PLANE('',#9909);
#1070=PLANE('',#9914);
#1071=PLANE('',#9923);
#1072=PLANE('',#9929);
#1073=PLANE('',#9931);
#1074=PLANE('',#9932);
#1075=PLANE('',#9933);
#1076=PLANE('',#9934);
#1077=PLANE('',#9935);
#1078=PLANE('',#9936);
#1079=PLANE('',#9937);
#1080=PLANE('',#9938);
#1081=PLANE('',#9946);
#1082=PLANE('',#9961);
#1083=PLANE('',#9962);
#1084=PLANE('',#9968);
#1085=PLANE('',#9975);
#1086=PLANE('',#9976);
#1087=PLANE('',#9980);
#1088=PLANE('',#9982);
#1089=PLANE('',#9983);
#1090=PLANE('',#9985);
#1091=PLANE('',#9991);
#1092=PLANE('',#9996);
#1093=PLANE('',#10000);
#1094=PLANE('',#10001);
#1095=PLANE('',#10009);
#1096=PLANE('',#10010);
#1097=PLANE('',#10012);
#1098=PLANE('',#10016);
#1099=PLANE('',#10023);
#1100=PLANE('',#10024);
#1101=PLANE('',#10029);
#1102=PLANE('',#10030);
#1103=PLANE('',#10033);
#1104=PLANE('',#10041);
#1105=PLANE('',#10042);
#1106=PLANE('',#10050);
#1107=PLANE('',#10051);
#1108=PLANE('',#10059);
#1109=PLANE('',#10060);
#1110=PLANE('',#10068);
#1111=PLANE('',#10069);
#1112=PLANE('',#10074);
#1113=PLANE('',#10075);
#1114=PLANE('',#10078);
#1115=PLANE('',#10086);
#1116=PLANE('',#10087);
#1117=PLANE('',#10095);
#1118=PLANE('',#10096);
#1119=PLANE('',#10104);
#1120=PLANE('',#10105);
#1121=PLANE('',#10113);
#1122=PLANE('',#10114);
#1123=PLANE('',#10116);
#1124=PLANE('',#10124);
#1125=PLANE('',#10132);
#1126=PLANE('',#10133);
#1127=PLANE('',#10134);
#1128=PLANE('',#10135);
#1129=PLANE('',#10136);
#1130=PLANE('',#10137);
#1131=PLANE('',#10138);
#1132=PLANE('',#10139);
#1133=PLANE('',#10140);
#1134=PLANE('',#10142);
#1135=PLANE('',#10144);
#1136=PLANE('',#10145);
#1137=PLANE('',#10146);
#1138=PLANE('',#10147);
#1139=PLANE('',#10148);
#1140=PLANE('',#10149);
#1141=PLANE('',#10150);
#1142=PLANE('',#10151);
#1143=PLANE('',#10167);
#1144=PLANE('',#10168);
#1145=PLANE('',#10170);
#1146=PLANE('',#10173);
#1147=PLANE('',#10181);
#1148=PLANE('',#10182);
#1149=PLANE('',#10190);
#1150=PLANE('',#10191);
#1151=PLANE('',#10206);
#1152=PLANE('',#10207);
#1153=PLANE('',#10209);
#1154=PLANE('',#10212);
#1155=PLANE('',#10220);
#1156=PLANE('',#10221);
#1157=PLANE('',#10229);
#1158=PLANE('',#10230);
#1159=PLANE('',#10239);
#1160=PLANE('',#10255);
#1161=PLANE('',#10256);
#1162=PLANE('',#10257);
#1163=PLANE('',#10258);
#1164=PLANE('',#10259);
#1165=PLANE('',#10260);
#1166=PLANE('',#10277);
#1167=PLANE('',#10278);
#1168=PLANE('',#10279);
#1169=PLANE('',#10280);
#1170=PLANE('',#10281);
#1171=PLANE('',#10282);
#1172=PLANE('',#10299);
#1173=PLANE('',#10300);
#1174=PLANE('',#10301);
#1175=PLANE('',#10302);
#1176=PLANE('',#10303);
#1177=PLANE('',#10304);
#1178=PLANE('',#10309);
#1179=PLANE('',#10310);
#1180=PLANE('',#10313);
#1181=PLANE('',#10321);
#1182=PLANE('',#10322);
#1183=PLANE('',#10330);
#1184=PLANE('',#10331);
#1185=PLANE('',#10339);
#1186=PLANE('',#10340);
#1187=PLANE('',#10348);
#1188=PLANE('',#10349);
#1189=PLANE('',#10355);
#1190=PLANE('',#10371);
#1191=PLANE('',#10372);
#1192=PLANE('',#10373);
#1193=PLANE('',#10374);
#1194=PLANE('',#10375);
#1195=PLANE('',#10376);
#1196=PLANE('',#10393);
#1197=PLANE('',#10394);
#1198=PLANE('',#10395);
#1199=PLANE('',#10396);
#1200=PLANE('',#10397);
#1201=PLANE('',#10398);
#1202=PLANE('',#10415);
#1203=PLANE('',#10416);
#1204=PLANE('',#10417);
#1205=PLANE('',#10418);
#1206=PLANE('',#10419);
#1207=PLANE('',#10420);
#1208=PLANE('',#10425);
#1209=PLANE('',#10426);
#1210=PLANE('',#10429);
#1211=PLANE('',#10437);
#1212=PLANE('',#10438);
#1213=PLANE('',#10446);
#1214=PLANE('',#10447);
#1215=PLANE('',#10455);
#1216=PLANE('',#10456);
#1217=PLANE('',#10464);
#1218=PLANE('',#10465);
#1219=PLANE('',#10468);
#1220=PLANE('',#10470);
#1221=PLANE('',#10471);
#1222=PLANE('',#10473);
#1223=PLANE('',#10474);
#1224=PLANE('',#10475);
#1225=PLANE('',#10480);
#1226=PLANE('',#10484);
#1227=PLANE('',#10488);
#1228=PLANE('',#10492);
#1229=PLANE('',#10496);
#1230=PLANE('',#10500);
#1231=PLANE('',#10503);
#1232=PLANE('',#10504);
#1233=PLANE('',#10507);
#1234=PLANE('',#10508);
#1235=PLANE('',#10513);
#1236=PLANE('',#10519);
#1237=PLANE('',#10520);
#1238=PLANE('',#10521);
#1239=PLANE('',#10522);
#1240=PLANE('',#10523);
#1241=PLANE('',#10524);
#1242=PLANE('',#10525);
#1243=PLANE('',#10526);
#1244=PLANE('',#10527);
#1245=PLANE('',#10529);
#1246=PLANE('',#10537);
#1247=FACE_OUTER_BOUND('',#1769,.T.);
#1248=FACE_OUTER_BOUND('',#1770,.T.);
#1249=FACE_OUTER_BOUND('',#1771,.T.);
#1250=FACE_OUTER_BOUND('',#1772,.T.);
#1251=FACE_OUTER_BOUND('',#1773,.T.);
#1252=FACE_OUTER_BOUND('',#1774,.T.);
#1253=FACE_OUTER_BOUND('',#1775,.T.);
#1254=FACE_OUTER_BOUND('',#1776,.T.);
#1255=FACE_OUTER_BOUND('',#1777,.T.);
#1256=FACE_OUTER_BOUND('',#1778,.T.);
#1257=FACE_OUTER_BOUND('',#1779,.T.);
#1258=FACE_OUTER_BOUND('',#1780,.T.);
#1259=FACE_OUTER_BOUND('',#1781,.T.);
#1260=FACE_OUTER_BOUND('',#1782,.T.);
#1261=FACE_OUTER_BOUND('',#1783,.T.);
#1262=FACE_OUTER_BOUND('',#1784,.T.);
#1263=FACE_OUTER_BOUND('',#1785,.T.);
#1264=FACE_OUTER_BOUND('',#1798,.T.);
#1265=FACE_OUTER_BOUND('',#1811,.T.);
#1266=FACE_OUTER_BOUND('',#1812,.T.);
#1267=FACE_OUTER_BOUND('',#1813,.T.);
#1268=FACE_OUTER_BOUND('',#1814,.T.);
#1269=FACE_OUTER_BOUND('',#1815,.T.);
#1270=FACE_OUTER_BOUND('',#1816,.T.);
#1271=FACE_OUTER_BOUND('',#1817,.T.);
#1272=FACE_OUTER_BOUND('',#1818,.T.);
#1273=FACE_OUTER_BOUND('',#1819,.T.);
#1274=FACE_OUTER_BOUND('',#1820,.T.);
#1275=FACE_OUTER_BOUND('',#1821,.T.);
#1276=FACE_OUTER_BOUND('',#1822,.T.);
#1277=FACE_OUTER_BOUND('',#1823,.T.);
#1278=FACE_OUTER_BOUND('',#1824,.T.);
#1279=FACE_OUTER_BOUND('',#1825,.T.);
#1280=FACE_OUTER_BOUND('',#1826,.T.);
#1281=FACE_OUTER_BOUND('',#1827,.T.);
#1282=FACE_OUTER_BOUND('',#1828,.T.);
#1283=FACE_OUTER_BOUND('',#1829,.T.);
#1284=FACE_OUTER_BOUND('',#1830,.T.);
#1285=FACE_OUTER_BOUND('',#1831,.T.);
#1286=FACE_OUTER_BOUND('',#1832,.T.);
#1287=FACE_OUTER_BOUND('',#1833,.T.);
#1288=FACE_OUTER_BOUND('',#1834,.T.);
#1289=FACE_OUTER_BOUND('',#1835,.T.);
#1290=FACE_OUTER_BOUND('',#1836,.T.);
#1291=FACE_OUTER_BOUND('',#1837,.T.);
#1292=FACE_OUTER_BOUND('',#1838,.T.);
#1293=FACE_OUTER_BOUND('',#1839,.T.);
#1294=FACE_OUTER_BOUND('',#1840,.T.);
#1295=FACE_OUTER_BOUND('',#1841,.T.);
#1296=FACE_OUTER_BOUND('',#1847,.T.);
#1297=FACE_OUTER_BOUND('',#1848,.T.);
#1298=FACE_OUTER_BOUND('',#1849,.T.);
#1299=FACE_OUTER_BOUND('',#1850,.T.);
#1300=FACE_OUTER_BOUND('',#1851,.T.);
#1301=FACE_OUTER_BOUND('',#1852,.T.);
#1302=FACE_OUTER_BOUND('',#1854,.T.);
#1303=FACE_OUTER_BOUND('',#1856,.T.);
#1304=FACE_OUTER_BOUND('',#1858,.T.);
#1305=FACE_OUTER_BOUND('',#1864,.T.);
#1306=FACE_OUTER_BOUND('',#1870,.T.);
#1307=FACE_OUTER_BOUND('',#1871,.T.);
#1308=FACE_OUTER_BOUND('',#1873,.T.);
#1309=FACE_OUTER_BOUND('',#1874,.T.);
#1310=FACE_OUTER_BOUND('',#1876,.T.);
#1311=FACE_OUTER_BOUND('',#1877,.T.);
#1312=FACE_OUTER_BOUND('',#1879,.T.);
#1313=FACE_OUTER_BOUND('',#1880,.T.);
#1314=FACE_OUTER_BOUND('',#1882,.T.);
#1315=FACE_OUTER_BOUND('',#1883,.T.);
#1316=FACE_OUTER_BOUND('',#1884,.T.);
#1317=FACE_OUTER_BOUND('',#1885,.T.);
#1318=FACE_OUTER_BOUND('',#1886,.T.);
#1319=FACE_OUTER_BOUND('',#1887,.T.);
#1320=FACE_OUTER_BOUND('',#1889,.T.);
#1321=FACE_OUTER_BOUND('',#1890,.T.);
#1322=FACE_OUTER_BOUND('',#1891,.T.);
#1323=FACE_OUTER_BOUND('',#1897,.T.);
#1324=FACE_OUTER_BOUND('',#1903,.T.);
#1325=FACE_OUTER_BOUND('',#1904,.T.);
#1326=FACE_OUTER_BOUND('',#1905,.T.);
#1327=FACE_OUTER_BOUND('',#1906,.T.);
#1328=FACE_OUTER_BOUND('',#1907,.T.);
#1329=FACE_OUTER_BOUND('',#1908,.T.);
#1330=FACE_OUTER_BOUND('',#1909,.T.);
#1331=FACE_OUTER_BOUND('',#1911,.T.);
#1332=FACE_OUTER_BOUND('',#1912,.T.);
#1333=FACE_OUTER_BOUND('',#1914,.T.);
#1334=FACE_OUTER_BOUND('',#1916,.T.);
#1335=FACE_OUTER_BOUND('',#1917,.T.);
#1336=FACE_OUTER_BOUND('',#1918,.T.);
#1337=FACE_OUTER_BOUND('',#1919,.T.);
#1338=FACE_OUTER_BOUND('',#1920,.T.);
#1339=FACE_OUTER_BOUND('',#1922,.T.);
#1340=FACE_OUTER_BOUND('',#1923,.T.);
#1341=FACE_OUTER_BOUND('',#1925,.T.);
#1342=FACE_OUTER_BOUND('',#1928,.T.);
#1343=FACE_OUTER_BOUND('',#1929,.T.);
#1344=FACE_OUTER_BOUND('',#1930,.T.);
#1345=FACE_OUTER_BOUND('',#1931,.T.);
#1346=FACE_OUTER_BOUND('',#1932,.T.);
#1347=FACE_OUTER_BOUND('',#1933,.T.);
#1348=FACE_OUTER_BOUND('',#1934,.T.);
#1349=FACE_OUTER_BOUND('',#1936,.T.);
#1350=FACE_OUTER_BOUND('',#1937,.T.);
#1351=FACE_OUTER_BOUND('',#1939,.T.);
#1352=FACE_OUTER_BOUND('',#1941,.T.);
#1353=FACE_OUTER_BOUND('',#1942,.T.);
#1354=FACE_OUTER_BOUND('',#1943,.T.);
#1355=FACE_OUTER_BOUND('',#1944,.T.);
#1356=FACE_OUTER_BOUND('',#1945,.T.);
#1357=FACE_OUTER_BOUND('',#1947,.T.);
#1358=FACE_OUTER_BOUND('',#1948,.T.);
#1359=FACE_OUTER_BOUND('',#1950,.T.);
#1360=FACE_OUTER_BOUND('',#1953,.T.);
#1361=FACE_OUTER_BOUND('',#1954,.T.);
#1362=FACE_OUTER_BOUND('',#1955,.T.);
#1363=FACE_OUTER_BOUND('',#1956,.T.);
#1364=FACE_OUTER_BOUND('',#1957,.T.);
#1365=FACE_OUTER_BOUND('',#1958,.T.);
#1366=FACE_OUTER_BOUND('',#1960,.T.);
#1367=FACE_OUTER_BOUND('',#1961,.T.);
#1368=FACE_OUTER_BOUND('',#1963,.T.);
#1369=FACE_OUTER_BOUND('',#1965,.T.);
#1370=FACE_OUTER_BOUND('',#1966,.T.);
#1371=FACE_OUTER_BOUND('',#1967,.T.);
#1372=FACE_OUTER_BOUND('',#1969,.T.);
#1373=FACE_OUTER_BOUND('',#1971,.T.);
#1374=FACE_OUTER_BOUND('',#1972,.T.);
#1375=FACE_OUTER_BOUND('',#1974,.T.);
#1376=FACE_OUTER_BOUND('',#1975,.T.);
#1377=FACE_OUTER_BOUND('',#1978,.T.);
#1378=FACE_OUTER_BOUND('',#1979,.T.);
#1379=FACE_OUTER_BOUND('',#1980,.T.);
#1380=FACE_OUTER_BOUND('',#1981,.T.);
#1381=FACE_OUTER_BOUND('',#1982,.T.);
#1382=FACE_OUTER_BOUND('',#1983,.T.);
#1383=FACE_OUTER_BOUND('',#1985,.T.);
#1384=FACE_OUTER_BOUND('',#1986,.T.);
#1385=FACE_OUTER_BOUND('',#1988,.T.);
#1386=FACE_OUTER_BOUND('',#1990,.T.);
#1387=FACE_OUTER_BOUND('',#1991,.T.);
#1388=FACE_OUTER_BOUND('',#1992,.T.);
#1389=FACE_OUTER_BOUND('',#1994,.T.);
#1390=FACE_OUTER_BOUND('',#1996,.T.);
#1391=FACE_OUTER_BOUND('',#1997,.T.);
#1392=FACE_OUTER_BOUND('',#1999,.T.);
#1393=FACE_OUTER_BOUND('',#2000,.T.);
#1394=FACE_OUTER_BOUND('',#2003,.T.);
#1395=FACE_OUTER_BOUND('',#2004,.T.);
#1396=FACE_OUTER_BOUND('',#2005,.T.);
#1397=FACE_OUTER_BOUND('',#2006,.T.);
#1398=FACE_OUTER_BOUND('',#2007,.T.);
#1399=FACE_OUTER_BOUND('',#2008,.T.);
#1400=FACE_OUTER_BOUND('',#2009,.T.);
#1401=FACE_OUTER_BOUND('',#2010,.T.);
#1402=FACE_OUTER_BOUND('',#2011,.T.);
#1403=FACE_OUTER_BOUND('',#2012,.T.);
#1404=FACE_OUTER_BOUND('',#2013,.T.);
#1405=FACE_OUTER_BOUND('',#2014,.T.);
#1406=FACE_OUTER_BOUND('',#2015,.T.);
#1407=FACE_OUTER_BOUND('',#2016,.T.);
#1408=FACE_OUTER_BOUND('',#2018,.T.);
#1409=FACE_OUTER_BOUND('',#2019,.T.);
#1410=FACE_OUTER_BOUND('',#2020,.T.);
#1411=FACE_OUTER_BOUND('',#2021,.T.);
#1412=FACE_OUTER_BOUND('',#2022,.T.);
#1413=FACE_OUTER_BOUND('',#2023,.T.);
#1414=FACE_OUTER_BOUND('',#2024,.T.);
#1415=FACE_OUTER_BOUND('',#2026,.T.);
#1416=FACE_OUTER_BOUND('',#2027,.T.);
#1417=FACE_OUTER_BOUND('',#2029,.T.);
#1418=FACE_OUTER_BOUND('',#2030,.T.);
#1419=FACE_OUTER_BOUND('',#2031,.T.);
#1420=FACE_OUTER_BOUND('',#2032,.T.);
#1421=FACE_OUTER_BOUND('',#2034,.T.);
#1422=FACE_OUTER_BOUND('',#2035,.T.);
#1423=FACE_OUTER_BOUND('',#2036,.T.);
#1424=FACE_OUTER_BOUND('',#2037,.T.);
#1425=FACE_OUTER_BOUND('',#2039,.T.);
#1426=FACE_OUTER_BOUND('',#2040,.T.);
#1427=FACE_OUTER_BOUND('',#2041,.T.);
#1428=FACE_OUTER_BOUND('',#2042,.T.);
#1429=FACE_OUTER_BOUND('',#2043,.T.);
#1430=FACE_OUTER_BOUND('',#2044,.T.);
#1431=FACE_OUTER_BOUND('',#2045,.T.);
#1432=FACE_OUTER_BOUND('',#2046,.T.);
#1433=FACE_OUTER_BOUND('',#2047,.T.);
#1434=FACE_OUTER_BOUND('',#2048,.T.);
#1435=FACE_OUTER_BOUND('',#2049,.T.);
#1436=FACE_OUTER_BOUND('',#2050,.T.);
#1437=FACE_OUTER_BOUND('',#2051,.T.);
#1438=FACE_OUTER_BOUND('',#2052,.T.);
#1439=FACE_OUTER_BOUND('',#2053,.T.);
#1440=FACE_OUTER_BOUND('',#2054,.T.);
#1441=FACE_OUTER_BOUND('',#2055,.T.);
#1442=FACE_OUTER_BOUND('',#2056,.T.);
#1443=FACE_OUTER_BOUND('',#2057,.T.);
#1444=FACE_OUTER_BOUND('',#2058,.T.);
#1445=FACE_OUTER_BOUND('',#2059,.T.);
#1446=FACE_OUTER_BOUND('',#2060,.T.);
#1447=FACE_OUTER_BOUND('',#2061,.T.);
#1448=FACE_OUTER_BOUND('',#2062,.T.);
#1449=FACE_OUTER_BOUND('',#2063,.T.);
#1450=FACE_OUTER_BOUND('',#2064,.T.);
#1451=FACE_OUTER_BOUND('',#2065,.T.);
#1452=FACE_OUTER_BOUND('',#2067,.T.);
#1453=FACE_OUTER_BOUND('',#2068,.T.);
#1454=FACE_OUTER_BOUND('',#2070,.T.);
#1455=FACE_OUTER_BOUND('',#2071,.T.);
#1456=FACE_OUTER_BOUND('',#2073,.T.);
#1457=FACE_OUTER_BOUND('',#2074,.T.);
#1458=FACE_OUTER_BOUND('',#2076,.T.);
#1459=FACE_OUTER_BOUND('',#2077,.T.);
#1460=FACE_OUTER_BOUND('',#2079,.T.);
#1461=FACE_OUTER_BOUND('',#2080,.T.);
#1462=FACE_OUTER_BOUND('',#2081,.T.);
#1463=FACE_OUTER_BOUND('',#2082,.T.);
#1464=FACE_OUTER_BOUND('',#2083,.T.);
#1465=FACE_OUTER_BOUND('',#2084,.T.);
#1466=FACE_OUTER_BOUND('',#2085,.T.);
#1467=FACE_OUTER_BOUND('',#2086,.T.);
#1468=FACE_OUTER_BOUND('',#2087,.T.);
#1469=FACE_OUTER_BOUND('',#2088,.T.);
#1470=FACE_OUTER_BOUND('',#2089,.T.);
#1471=FACE_OUTER_BOUND('',#2090,.T.);
#1472=FACE_OUTER_BOUND('',#2091,.T.);
#1473=FACE_OUTER_BOUND('',#2093,.T.);
#1474=FACE_OUTER_BOUND('',#2094,.T.);
#1475=FACE_OUTER_BOUND('',#2095,.T.);
#1476=FACE_OUTER_BOUND('',#2096,.T.);
#1477=FACE_OUTER_BOUND('',#2097,.T.);
#1478=FACE_OUTER_BOUND('',#2098,.T.);
#1479=FACE_OUTER_BOUND('',#2099,.T.);
#1480=FACE_OUTER_BOUND('',#2100,.T.);
#1481=FACE_OUTER_BOUND('',#2101,.T.);
#1482=FACE_OUTER_BOUND('',#2102,.T.);
#1483=FACE_OUTER_BOUND('',#2106,.T.);
#1484=FACE_OUTER_BOUND('',#2107,.T.);
#1485=FACE_OUTER_BOUND('',#2108,.T.);
#1486=FACE_OUTER_BOUND('',#2109,.T.);
#1487=FACE_OUTER_BOUND('',#2110,.T.);
#1488=FACE_OUTER_BOUND('',#2111,.T.);
#1489=FACE_OUTER_BOUND('',#2116,.T.);
#1490=FACE_OUTER_BOUND('',#2117,.T.);
#1491=FACE_OUTER_BOUND('',#2118,.T.);
#1492=FACE_OUTER_BOUND('',#2119,.T.);
#1493=FACE_OUTER_BOUND('',#2120,.T.);
#1494=FACE_OUTER_BOUND('',#2121,.T.);
#1495=FACE_OUTER_BOUND('',#2123,.T.);
#1496=FACE_OUTER_BOUND('',#2124,.T.);
#1497=FACE_OUTER_BOUND('',#2125,.T.);
#1498=FACE_OUTER_BOUND('',#2126,.T.);
#1499=FACE_OUTER_BOUND('',#2127,.T.);
#1500=FACE_OUTER_BOUND('',#2128,.T.);
#1501=FACE_OUTER_BOUND('',#2129,.T.);
#1502=FACE_OUTER_BOUND('',#2130,.T.);
#1503=FACE_OUTER_BOUND('',#2132,.T.);
#1504=FACE_OUTER_BOUND('',#2133,.T.);
#1505=FACE_OUTER_BOUND('',#2134,.T.);
#1506=FACE_OUTER_BOUND('',#2136,.T.);
#1507=FACE_OUTER_BOUND('',#2138,.T.);
#1508=FACE_OUTER_BOUND('',#2139,.T.);
#1509=FACE_OUTER_BOUND('',#2140,.T.);
#1510=FACE_OUTER_BOUND('',#2141,.T.);
#1511=FACE_OUTER_BOUND('',#2143,.T.);
#1512=FACE_OUTER_BOUND('',#2145,.T.);
#1513=FACE_OUTER_BOUND('',#2147,.T.);
#1514=FACE_OUTER_BOUND('',#2149,.T.);
#1515=FACE_OUTER_BOUND('',#2150,.T.);
#1516=FACE_OUTER_BOUND('',#2151,.T.);
#1517=FACE_OUTER_BOUND('',#2153,.T.);
#1518=FACE_OUTER_BOUND('',#2155,.T.);
#1519=FACE_OUTER_BOUND('',#2156,.T.);
#1520=FACE_OUTER_BOUND('',#2157,.T.);
#1521=FACE_OUTER_BOUND('',#2158,.T.);
#1522=FACE_OUTER_BOUND('',#2160,.T.);
#1523=FACE_OUTER_BOUND('',#2161,.T.);
#1524=FACE_OUTER_BOUND('',#2162,.T.);
#1525=FACE_OUTER_BOUND('',#2163,.T.);
#1526=FACE_OUTER_BOUND('',#2165,.T.);
#1527=FACE_OUTER_BOUND('',#2167,.T.);
#1528=FACE_OUTER_BOUND('',#2168,.T.);
#1529=FACE_OUTER_BOUND('',#2169,.T.);
#1530=FACE_OUTER_BOUND('',#2171,.T.);
#1531=FACE_OUTER_BOUND('',#2173,.T.);
#1532=FACE_OUTER_BOUND('',#2174,.T.);
#1533=FACE_OUTER_BOUND('',#2175,.T.);
#1534=FACE_OUTER_BOUND('',#2177,.T.);
#1535=FACE_OUTER_BOUND('',#2179,.T.);
#1536=FACE_OUTER_BOUND('',#2180,.T.);
#1537=FACE_OUTER_BOUND('',#2181,.T.);
#1538=FACE_OUTER_BOUND('',#2183,.T.);
#1539=FACE_OUTER_BOUND('',#2185,.T.);
#1540=FACE_OUTER_BOUND('',#2186,.T.);
#1541=FACE_OUTER_BOUND('',#2187,.T.);
#1542=FACE_OUTER_BOUND('',#2188,.T.);
#1543=FACE_OUTER_BOUND('',#2190,.T.);
#1544=FACE_OUTER_BOUND('',#2191,.T.);
#1545=FACE_OUTER_BOUND('',#2192,.T.);
#1546=FACE_OUTER_BOUND('',#2193,.T.);
#1547=FACE_OUTER_BOUND('',#2195,.T.);
#1548=FACE_OUTER_BOUND('',#2197,.T.);
#1549=FACE_OUTER_BOUND('',#2198,.T.);
#1550=FACE_OUTER_BOUND('',#2199,.T.);
#1551=FACE_OUTER_BOUND('',#2201,.T.);
#1552=FACE_OUTER_BOUND('',#2203,.T.);
#1553=FACE_OUTER_BOUND('',#2204,.T.);
#1554=FACE_OUTER_BOUND('',#2205,.T.);
#1555=FACE_OUTER_BOUND('',#2207,.T.);
#1556=FACE_OUTER_BOUND('',#2209,.T.);
#1557=FACE_OUTER_BOUND('',#2210,.T.);
#1558=FACE_OUTER_BOUND('',#2211,.T.);
#1559=FACE_OUTER_BOUND('',#2212,.T.);
#1560=FACE_OUTER_BOUND('',#2213,.T.);
#1561=FACE_OUTER_BOUND('',#2215,.T.);
#1562=FACE_OUTER_BOUND('',#2216,.T.);
#1563=FACE_OUTER_BOUND('',#2217,.T.);
#1564=FACE_OUTER_BOUND('',#2218,.T.);
#1565=FACE_OUTER_BOUND('',#2219,.T.);
#1566=FACE_OUTER_BOUND('',#2220,.T.);
#1567=FACE_OUTER_BOUND('',#2221,.T.);
#1568=FACE_OUTER_BOUND('',#2222,.T.);
#1569=FACE_OUTER_BOUND('',#2223,.T.);
#1570=FACE_OUTER_BOUND('',#2224,.T.);
#1571=FACE_OUTER_BOUND('',#2225,.T.);
#1572=FACE_OUTER_BOUND('',#2226,.T.);
#1573=FACE_OUTER_BOUND('',#2227,.T.);
#1574=FACE_OUTER_BOUND('',#2228,.T.);
#1575=FACE_OUTER_BOUND('',#2229,.T.);
#1576=FACE_OUTER_BOUND('',#2230,.T.);
#1577=FACE_OUTER_BOUND('',#2231,.T.);
#1578=FACE_OUTER_BOUND('',#2232,.T.);
#1579=FACE_OUTER_BOUND('',#2233,.T.);
#1580=FACE_OUTER_BOUND('',#2234,.T.);
#1581=FACE_OUTER_BOUND('',#2235,.T.);
#1582=FACE_OUTER_BOUND('',#2237,.T.);
#1583=FACE_OUTER_BOUND('',#2238,.T.);
#1584=FACE_OUTER_BOUND('',#2239,.T.);
#1585=FACE_OUTER_BOUND('',#2240,.T.);
#1586=FACE_OUTER_BOUND('',#2241,.T.);
#1587=FACE_OUTER_BOUND('',#2242,.T.);
#1588=FACE_OUTER_BOUND('',#2243,.T.);
#1589=FACE_OUTER_BOUND('',#2246,.T.);
#1590=FACE_OUTER_BOUND('',#2247,.T.);
#1591=FACE_OUTER_BOUND('',#2248,.T.);
#1592=FACE_OUTER_BOUND('',#2251,.T.);
#1593=FACE_OUTER_BOUND('',#2252,.T.);
#1594=FACE_OUTER_BOUND('',#2253,.T.);
#1595=FACE_OUTER_BOUND('',#2255,.T.);
#1596=FACE_OUTER_BOUND('',#2257,.T.);
#1597=FACE_OUTER_BOUND('',#2258,.T.);
#1598=FACE_OUTER_BOUND('',#2259,.T.);
#1599=FACE_OUTER_BOUND('',#2261,.T.);
#1600=FACE_OUTER_BOUND('',#2263,.T.);
#1601=FACE_OUTER_BOUND('',#2264,.T.);
#1602=FACE_OUTER_BOUND('',#2265,.T.);
#1603=FACE_OUTER_BOUND('',#2266,.T.);
#1604=FACE_OUTER_BOUND('',#2267,.T.);
#1605=FACE_OUTER_BOUND('',#2270,.T.);
#1606=FACE_OUTER_BOUND('',#2271,.T.);
#1607=FACE_OUTER_BOUND('',#2272,.T.);
#1608=FACE_OUTER_BOUND('',#2275,.T.);
#1609=FACE_OUTER_BOUND('',#2276,.T.);
#1610=FACE_OUTER_BOUND('',#2277,.T.);
#1611=FACE_OUTER_BOUND('',#2279,.T.);
#1612=FACE_OUTER_BOUND('',#2281,.T.);
#1613=FACE_OUTER_BOUND('',#2282,.T.);
#1614=FACE_OUTER_BOUND('',#2283,.T.);
#1615=FACE_OUTER_BOUND('',#2285,.T.);
#1616=FACE_OUTER_BOUND('',#2287,.T.);
#1617=FACE_OUTER_BOUND('',#2288,.T.);
#1618=FACE_OUTER_BOUND('',#2289,.T.);
#1619=FACE_OUTER_BOUND('',#2290,.T.);
#1620=FACE_OUTER_BOUND('',#2291,.T.);
#1621=FACE_OUTER_BOUND('',#2292,.T.);
#1622=FACE_OUTER_BOUND('',#2293,.T.);
#1623=FACE_OUTER_BOUND('',#2294,.T.);
#1624=FACE_OUTER_BOUND('',#2295,.T.);
#1625=FACE_OUTER_BOUND('',#2301,.T.);
#1626=FACE_OUTER_BOUND('',#2302,.T.);
#1627=FACE_OUTER_BOUND('',#2308,.T.);
#1628=FACE_OUTER_BOUND('',#2310,.T.);
#1629=FACE_OUTER_BOUND('',#2311,.T.);
#1630=FACE_OUTER_BOUND('',#2312,.T.);
#1631=FACE_OUTER_BOUND('',#2313,.T.);
#1632=FACE_OUTER_BOUND('',#2314,.T.);
#1633=FACE_OUTER_BOUND('',#2315,.T.);
#1634=FACE_OUTER_BOUND('',#2316,.T.);
#1635=FACE_OUTER_BOUND('',#2317,.T.);
#1636=FACE_OUTER_BOUND('',#2323,.T.);
#1637=FACE_OUTER_BOUND('',#2324,.T.);
#1638=FACE_OUTER_BOUND('',#2330,.T.);
#1639=FACE_OUTER_BOUND('',#2331,.T.);
#1640=FACE_OUTER_BOUND('',#2332,.T.);
#1641=FACE_OUTER_BOUND('',#2333,.T.);
#1642=FACE_OUTER_BOUND('',#2334,.T.);
#1643=FACE_OUTER_BOUND('',#2335,.T.);
#1644=FACE_OUTER_BOUND('',#2336,.T.);
#1645=FACE_OUTER_BOUND('',#2337,.T.);
#1646=FACE_OUTER_BOUND('',#2338,.T.);
#1647=FACE_OUTER_BOUND('',#2344,.T.);
#1648=FACE_OUTER_BOUND('',#2345,.T.);
#1649=FACE_OUTER_BOUND('',#2351,.T.);
#1650=FACE_OUTER_BOUND('',#2352,.T.);
#1651=FACE_OUTER_BOUND('',#2353,.T.);
#1652=FACE_OUTER_BOUND('',#2354,.T.);
#1653=FACE_OUTER_BOUND('',#2355,.T.);
#1654=FACE_OUTER_BOUND('',#2357,.T.);
#1655=FACE_OUTER_BOUND('',#2359,.T.);
#1656=FACE_OUTER_BOUND('',#2360,.T.);
#1657=FACE_OUTER_BOUND('',#2361,.T.);
#1658=FACE_OUTER_BOUND('',#2362,.T.);
#1659=FACE_OUTER_BOUND('',#2364,.T.);
#1660=FACE_OUTER_BOUND('',#2365,.T.);
#1661=FACE_OUTER_BOUND('',#2366,.T.);
#1662=FACE_OUTER_BOUND('',#2367,.T.);
#1663=FACE_OUTER_BOUND('',#2369,.T.);
#1664=FACE_OUTER_BOUND('',#2371,.T.);
#1665=FACE_OUTER_BOUND('',#2372,.T.);
#1666=FACE_OUTER_BOUND('',#2373,.T.);
#1667=FACE_OUTER_BOUND('',#2375,.T.);
#1668=FACE_OUTER_BOUND('',#2377,.T.);
#1669=FACE_OUTER_BOUND('',#2378,.T.);
#1670=FACE_OUTER_BOUND('',#2379,.T.);
#1671=FACE_OUTER_BOUND('',#2381,.T.);
#1672=FACE_OUTER_BOUND('',#2383,.T.);
#1673=FACE_OUTER_BOUND('',#2384,.T.);
#1674=FACE_OUTER_BOUND('',#2385,.T.);
#1675=FACE_OUTER_BOUND('',#2386,.T.);
#1676=FACE_OUTER_BOUND('',#2387,.T.);
#1677=FACE_OUTER_BOUND('',#2388,.T.);
#1678=FACE_OUTER_BOUND('',#2389,.T.);
#1679=FACE_OUTER_BOUND('',#2390,.T.);
#1680=FACE_OUTER_BOUND('',#2396,.T.);
#1681=FACE_OUTER_BOUND('',#2397,.T.);
#1682=FACE_OUTER_BOUND('',#2403,.T.);
#1683=FACE_OUTER_BOUND('',#2404,.T.);
#1684=FACE_OUTER_BOUND('',#2406,.T.);
#1685=FACE_OUTER_BOUND('',#2407,.T.);
#1686=FACE_OUTER_BOUND('',#2408,.T.);
#1687=FACE_OUTER_BOUND('',#2409,.T.);
#1688=FACE_OUTER_BOUND('',#2410,.T.);
#1689=FACE_OUTER_BOUND('',#2411,.T.);
#1690=FACE_OUTER_BOUND('',#2412,.T.);
#1691=FACE_OUTER_BOUND('',#2418,.T.);
#1692=FACE_OUTER_BOUND('',#2419,.T.);
#1693=FACE_OUTER_BOUND('',#2425,.T.);
#1694=FACE_OUTER_BOUND('',#2426,.T.);
#1695=FACE_OUTER_BOUND('',#2427,.T.);
#1696=FACE_OUTER_BOUND('',#2428,.T.);
#1697=FACE_OUTER_BOUND('',#2429,.T.);
#1698=FACE_OUTER_BOUND('',#2430,.T.);
#1699=FACE_OUTER_BOUND('',#2431,.T.);
#1700=FACE_OUTER_BOUND('',#2432,.T.);
#1701=FACE_OUTER_BOUND('',#2433,.T.);
#1702=FACE_OUTER_BOUND('',#2439,.T.);
#1703=FACE_OUTER_BOUND('',#2440,.T.);
#1704=FACE_OUTER_BOUND('',#2446,.T.);
#1705=FACE_OUTER_BOUND('',#2447,.T.);
#1706=FACE_OUTER_BOUND('',#2448,.T.);
#1707=FACE_OUTER_BOUND('',#2449,.T.);
#1708=FACE_OUTER_BOUND('',#2450,.T.);
#1709=FACE_OUTER_BOUND('',#2451,.T.);
#1710=FACE_OUTER_BOUND('',#2453,.T.);
#1711=FACE_OUTER_BOUND('',#2455,.T.);
#1712=FACE_OUTER_BOUND('',#2456,.T.);
#1713=FACE_OUTER_BOUND('',#2457,.T.);
#1714=FACE_OUTER_BOUND('',#2458,.T.);
#1715=FACE_OUTER_BOUND('',#2460,.T.);
#1716=FACE_OUTER_BOUND('',#2461,.T.);
#1717=FACE_OUTER_BOUND('',#2462,.T.);
#1718=FACE_OUTER_BOUND('',#2463,.T.);
#1719=FACE_OUTER_BOUND('',#2465,.T.);
#1720=FACE_OUTER_BOUND('',#2467,.T.);
#1721=FACE_OUTER_BOUND('',#2468,.T.);
#1722=FACE_OUTER_BOUND('',#2469,.T.);
#1723=FACE_OUTER_BOUND('',#2471,.T.);
#1724=FACE_OUTER_BOUND('',#2473,.T.);
#1725=FACE_OUTER_BOUND('',#2474,.T.);
#1726=FACE_OUTER_BOUND('',#2475,.T.);
#1727=FACE_OUTER_BOUND('',#2477,.T.);
#1728=FACE_OUTER_BOUND('',#2479,.T.);
#1729=FACE_OUTER_BOUND('',#2480,.T.);
#1730=FACE_OUTER_BOUND('',#2481,.T.);
#1731=FACE_OUTER_BOUND('',#2482,.T.);
#1732=FACE_OUTER_BOUND('',#2483,.T.);
#1733=FACE_OUTER_BOUND('',#2484,.T.);
#1734=FACE_OUTER_BOUND('',#2486,.T.);
#1735=FACE_OUTER_BOUND('',#2487,.T.);
#1736=FACE_OUTER_BOUND('',#2489,.T.);
#1737=FACE_OUTER_BOUND('',#2490,.T.);
#1738=FACE_OUTER_BOUND('',#2492,.T.);
#1739=FACE_OUTER_BOUND('',#2493,.T.);
#1740=FACE_OUTER_BOUND('',#2495,.T.);
#1741=FACE_OUTER_BOUND('',#2496,.T.);
#1742=FACE_OUTER_BOUND('',#2498,.T.);
#1743=FACE_OUTER_BOUND('',#2499,.T.);
#1744=FACE_OUTER_BOUND('',#2501,.T.);
#1745=FACE_OUTER_BOUND('',#2503,.T.);
#1746=FACE_OUTER_BOUND('',#2504,.T.);
#1747=FACE_OUTER_BOUND('',#2505,.T.);
#1748=FACE_OUTER_BOUND('',#2506,.T.);
#1749=FACE_OUTER_BOUND('',#2507,.T.);
#1750=FACE_OUTER_BOUND('',#2509,.T.);
#1751=FACE_OUTER_BOUND('',#2511,.T.);
#1752=FACE_OUTER_BOUND('',#2513,.T.);
#1753=FACE_OUTER_BOUND('',#2515,.T.);
#1754=FACE_OUTER_BOUND('',#2516,.T.);
#1755=FACE_OUTER_BOUND('',#2517,.T.);
#1756=FACE_OUTER_BOUND('',#2518,.T.);
#1757=FACE_OUTER_BOUND('',#2519,.T.);
#1758=FACE_OUTER_BOUND('',#2520,.T.);
#1759=FACE_OUTER_BOUND('',#2521,.T.);
#1760=FACE_OUTER_BOUND('',#2522,.T.);
#1761=FACE_OUTER_BOUND('',#2523,.T.);
#1762=FACE_OUTER_BOUND('',#2524,.T.);
#1763=FACE_OUTER_BOUND('',#2525,.T.);
#1764=FACE_OUTER_BOUND('',#2526,.T.);
#1765=FACE_OUTER_BOUND('',#2527,.T.);
#1766=FACE_OUTER_BOUND('',#2528,.T.);
#1767=FACE_OUTER_BOUND('',#2530,.T.);
#1768=FACE_OUTER_BOUND('',#2531,.T.);
#1769=EDGE_LOOP('',(#5911,#5912,#5913,#5914));
#1770=EDGE_LOOP('',(#5915,#5916,#5917,#5918));
#1771=EDGE_LOOP('',(#5919,#5920,#5921,#5922));
#1772=EDGE_LOOP('',(#5923,#5924,#5925,#5926));
#1773=EDGE_LOOP('',(#5927,#5928,#5929,#5930));
#1774=EDGE_LOOP('',(#5931,#5932,#5933,#5934));
#1775=EDGE_LOOP('',(#5935,#5936,#5937,#5938));
#1776=EDGE_LOOP('',(#5939,#5940,#5941,#5942));
#1777=EDGE_LOOP('',(#5943,#5944,#5945,#5946));
#1778=EDGE_LOOP('',(#5947,#5948,#5949,#5950));
#1779=EDGE_LOOP('',(#5951,#5952,#5953,#5954));
#1780=EDGE_LOOP('',(#5955,#5956,#5957,#5958));
#1781=EDGE_LOOP('',(#5959,#5960,#5961,#5962));
#1782=EDGE_LOOP('',(#5963,#5964,#5965,#5966));
#1783=EDGE_LOOP('',(#5967,#5968,#5969,#5970));
#1784=EDGE_LOOP('',(#5971,#5972,#5973,#5974));
#1785=EDGE_LOOP('',(#5975,#5976,#5977,#5978));
#1786=EDGE_LOOP('',(#5979));
#1787=EDGE_LOOP('',(#5980));
#1788=EDGE_LOOP('',(#5981));
#1789=EDGE_LOOP('',(#5982));
#1790=EDGE_LOOP('',(#5983));
#1791=EDGE_LOOP('',(#5984));
#1792=EDGE_LOOP('',(#5985));
#1793=EDGE_LOOP('',(#5986));
#1794=EDGE_LOOP('',(#5987));
#1795=EDGE_LOOP('',(#5988));
#1796=EDGE_LOOP('',(#5989));
#1797=EDGE_LOOP('',(#5990));
#1798=EDGE_LOOP('',(#5991,#5992,#5993,#5994));
#1799=EDGE_LOOP('',(#5995));
#1800=EDGE_LOOP('',(#5996));
#1801=EDGE_LOOP('',(#5997));
#1802=EDGE_LOOP('',(#5998));
#1803=EDGE_LOOP('',(#5999));
#1804=EDGE_LOOP('',(#6000));
#1805=EDGE_LOOP('',(#6001));
#1806=EDGE_LOOP('',(#6002));
#1807=EDGE_LOOP('',(#6003));
#1808=EDGE_LOOP('',(#6004));
#1809=EDGE_LOOP('',(#6005));
#1810=EDGE_LOOP('',(#6006));
#1811=EDGE_LOOP('',(#6007,#6008,#6009,#6010));
#1812=EDGE_LOOP('',(#6011,#6012,#6013,#6014));
#1813=EDGE_LOOP('',(#6015,#6016,#6017,#6018));
#1814=EDGE_LOOP('',(#6019,#6020,#6021,#6022));
#1815=EDGE_LOOP('',(#6023,#6024,#6025,#6026));
#1816=EDGE_LOOP('',(#6027,#6028,#6029,#6030));
#1817=EDGE_LOOP('',(#6031,#6032,#6033,#6034));
#1818=EDGE_LOOP('',(#6035,#6036,#6037,#6038));
#1819=EDGE_LOOP('',(#6039,#6040,#6041,#6042));
#1820=EDGE_LOOP('',(#6043,#6044,#6045,#6046));
#1821=EDGE_LOOP('',(#6047,#6048,#6049,#6050));
#1822=EDGE_LOOP('',(#6051,#6052,#6053,#6054));
#1823=EDGE_LOOP('',(#6055,#6056,#6057,#6058,#6059,#6060));
#1824=EDGE_LOOP('',(#6061,#6062,#6063,#6064));
#1825=EDGE_LOOP('',(#6065));
#1826=EDGE_LOOP('',(#6066,#6067,#6068,#6069));
#1827=EDGE_LOOP('',(#6070));
#1828=EDGE_LOOP('',(#6071,#6072,#6073,#6074));
#1829=EDGE_LOOP('',(#6075));
#1830=EDGE_LOOP('',(#6076,#6077,#6078,#6079));
#1831=EDGE_LOOP('',(#6080));
#1832=EDGE_LOOP('',(#6081,#6082));
#1833=EDGE_LOOP('',(#6083,#6084,#6085,#6086));
#1834=EDGE_LOOP('',(#6087,#6088,#6089,#6090));
#1835=EDGE_LOOP('',(#6091,#6092));
#1836=EDGE_LOOP('',(#6093,#6094,#6095,#6096));
#1837=EDGE_LOOP('',(#6097,#6098));
#1838=EDGE_LOOP('',(#6099,#6100,#6101,#6102));
#1839=EDGE_LOOP('',(#6103,#6104));
#1840=EDGE_LOOP('',(#6105,#6106,#6107,#6108,#6109,#6110,#6111,#6112,#6113,
#6114,#6115,#6116,#6117,#6118,#6119,#6120,#6121,#6122,#6123,#6124));
#1841=EDGE_LOOP('',(#6125));
#1842=EDGE_LOOP('',(#6126,#6127,#6128,#6129,#6130,#6131,#6132,#6133,#6134));
#1843=EDGE_LOOP('',(#6135));
#1844=EDGE_LOOP('',(#6136));
#1845=EDGE_LOOP('',(#6137));
#1846=EDGE_LOOP('',(#6138));
#1847=EDGE_LOOP('',(#6139,#6140,#6141,#6142));
#1848=EDGE_LOOP('',(#6143,#6144,#6145,#6146));
#1849=EDGE_LOOP('',(#6147,#6148,#6149,#6150));
#1850=EDGE_LOOP('',(#6151,#6152,#6153,#6154));
#1851=EDGE_LOOP('',(#6155,#6156,#6157,#6158));
#1852=EDGE_LOOP('',(#6159));
#1853=EDGE_LOOP('',(#6160));
#1854=EDGE_LOOP('',(#6161,#6162,#6163,#6164));
#1855=EDGE_LOOP('',(#6165,#6166));
#1856=EDGE_LOOP('',(#6167,#6168,#6169,#6170));
#1857=EDGE_LOOP('',(#6171,#6172));
#1858=EDGE_LOOP('',(#6173));
#1859=EDGE_LOOP('',(#6174));
#1860=EDGE_LOOP('',(#6175));
#1861=EDGE_LOOP('',(#6176));
#1862=EDGE_LOOP('',(#6177));
#1863=EDGE_LOOP('',(#6178));
#1864=EDGE_LOOP('',(#6179));
#1865=EDGE_LOOP('',(#6180));
#1866=EDGE_LOOP('',(#6181));
#1867=EDGE_LOOP('',(#6182));
#1868=EDGE_LOOP('',(#6183));
#1869=EDGE_LOOP('',(#6184));
#1870=EDGE_LOOP('',(#6185,#6186,#6187,#6188));
#1871=EDGE_LOOP('',(#6189));
#1872=EDGE_LOOP('',(#6190));
#1873=EDGE_LOOP('',(#6191,#6192,#6193,#6194));
#1874=EDGE_LOOP('',(#6195));
#1875=EDGE_LOOP('',(#6196));
#1876=EDGE_LOOP('',(#6197,#6198,#6199,#6200));
#1877=EDGE_LOOP('',(#6201));
#1878=EDGE_LOOP('',(#6202));
#1879=EDGE_LOOP('',(#6203,#6204,#6205,#6206));
#1880=EDGE_LOOP('',(#6207));
#1881=EDGE_LOOP('',(#6208));
#1882=EDGE_LOOP('',(#6209,#6210,#6211,#6212));
#1883=EDGE_LOOP('',(#6213,#6214,#6215,#6216));
#1884=EDGE_LOOP('',(#6217,#6218,#6219,#6220));
#1885=EDGE_LOOP('',(#6221,#6222,#6223,#6224));
#1886=EDGE_LOOP('',(#6225,#6226,#6227,#6228));
#1887=EDGE_LOOP('',(#6229));
#1888=EDGE_LOOP('',(#6230));
#1889=EDGE_LOOP('',(#6231,#6232,#6233,#6234));
#1890=EDGE_LOOP('',(#6235,#6236,#6237,#6238));
#1891=EDGE_LOOP('',(#6239));
#1892=EDGE_LOOP('',(#6240));
#1893=EDGE_LOOP('',(#6241));
#1894=EDGE_LOOP('',(#6242));
#1895=EDGE_LOOP('',(#6243));
#1896=EDGE_LOOP('',(#6244));
#1897=EDGE_LOOP('',(#6245));
#1898=EDGE_LOOP('',(#6246));
#1899=EDGE_LOOP('',(#6247));
#1900=EDGE_LOOP('',(#6248));
#1901=EDGE_LOOP('',(#6249));
#1902=EDGE_LOOP('',(#6250));
#1903=EDGE_LOOP('',(#6251,#6252,#6253,#6254));
#1904=EDGE_LOOP('',(#6255,#6256,#6257,#6258));
#1905=EDGE_LOOP('',(#6259,#6260));
#1906=EDGE_LOOP('',(#6261,#6262,#6263,#6264,#6265,#6266,#6267,#6268,#6269));
#1907=EDGE_LOOP('',(#6270,#6271));
#1908=EDGE_LOOP('',(#6272,#6273,#6274,#6275));
#1909=EDGE_LOOP('',(#6276,#6277));
#1910=EDGE_LOOP('',(#6278));
#1911=EDGE_LOOP('',(#6279,#6280,#6281,#6282));
#1912=EDGE_LOOP('',(#6283,#6284));
#1913=EDGE_LOOP('',(#6285));
#1914=EDGE_LOOP('',(#6286,#6287,#6288,#6289,#6290,#6291,#6292,#6293,#6294,
#6295));
#1915=EDGE_LOOP('',(#6296));
#1916=EDGE_LOOP('',(#6297,#6298,#6299,#6300));
#1917=EDGE_LOOP('',(#6301,#6302,#6303,#6304));
#1918=EDGE_LOOP('',(#6305,#6306,#6307,#6308,#6309,#6310,#6311,#6312,#6313,
#6314,#6315,#6316));
#1919=EDGE_LOOP('',(#6317,#6318,#6319,#6320,#6321,#6322,#6323));
#1920=EDGE_LOOP('',(#6324,#6325,#6326,#6327));
#1921=EDGE_LOOP('',(#6328));
#1922=EDGE_LOOP('',(#6329,#6330,#6331,#6332,#6333,#6334,#6335));
#1923=EDGE_LOOP('',(#6336,#6337,#6338,#6339));
#1924=EDGE_LOOP('',(#6340));
#1925=EDGE_LOOP('',(#6341,#6342,#6343,#6344));
#1926=EDGE_LOOP('',(#6345));
#1927=EDGE_LOOP('',(#6346));
#1928=EDGE_LOOP('',(#6347,#6348,#6349,#6350));
#1929=EDGE_LOOP('',(#6351,#6352,#6353,#6354));
#1930=EDGE_LOOP('',(#6355,#6356));
#1931=EDGE_LOOP('',(#6357,#6358,#6359,#6360,#6361,#6362,#6363,#6364,#6365));
#1932=EDGE_LOOP('',(#6366,#6367));
#1933=EDGE_LOOP('',(#6368,#6369,#6370,#6371));
#1934=EDGE_LOOP('',(#6372,#6373));
#1935=EDGE_LOOP('',(#6374));
#1936=EDGE_LOOP('',(#6375,#6376,#6377,#6378));
#1937=EDGE_LOOP('',(#6379,#6380));
#1938=EDGE_LOOP('',(#6381));
#1939=EDGE_LOOP('',(#6382,#6383,#6384,#6385,#6386,#6387,#6388,#6389,#6390,
#6391));
#1940=EDGE_LOOP('',(#6392));
#1941=EDGE_LOOP('',(#6393,#6394,#6395,#6396));
#1942=EDGE_LOOP('',(#6397,#6398,#6399,#6400));
#1943=EDGE_LOOP('',(#6401,#6402,#6403,#6404,#6405,#6406,#6407,#6408,#6409,
#6410,#6411,#6412));
#1944=EDGE_LOOP('',(#6413,#6414,#6415,#6416,#6417,#6418,#6419));
#1945=EDGE_LOOP('',(#6420,#6421,#6422,#6423));
#1946=EDGE_LOOP('',(#6424));
#1947=EDGE_LOOP('',(#6425,#6426,#6427,#6428,#6429,#6430,#6431));
#1948=EDGE_LOOP('',(#6432,#6433,#6434,#6435));
#1949=EDGE_LOOP('',(#6436));
#1950=EDGE_LOOP('',(#6437,#6438,#6439,#6440));
#1951=EDGE_LOOP('',(#6441));
#1952=EDGE_LOOP('',(#6442));
#1953=EDGE_LOOP('',(#6443,#6444,#6445,#6446));
#1954=EDGE_LOOP('',(#6447,#6448));
#1955=EDGE_LOOP('',(#6449,#6450,#6451,#6452,#6453,#6454,#6455,#6456));
#1956=EDGE_LOOP('',(#6457,#6458,#6459));
#1957=EDGE_LOOP('',(#6460,#6461,#6462,#6463));
#1958=EDGE_LOOP('',(#6464));
#1959=EDGE_LOOP('',(#6465));
#1960=EDGE_LOOP('',(#6466,#6467,#6468,#6469));
#1961=EDGE_LOOP('',(#6470,#6471));
#1962=EDGE_LOOP('',(#6472));
#1963=EDGE_LOOP('',(#6473,#6474,#6475,#6476,#6477,#6478,#6479,#6480,#6481));
#1964=EDGE_LOOP('',(#6482));
#1965=EDGE_LOOP('',(#6483,#6484,#6485,#6486));
#1966=EDGE_LOOP('',(#6487,#6488,#6489,#6490));
#1967=EDGE_LOOP('',(#6491,#6492,#6493,#6494));
#1968=EDGE_LOOP('',(#6495,#6496,#6497,#6498));
#1969=EDGE_LOOP('',(#6499,#6500,#6501,#6502));
#1970=EDGE_LOOP('',(#6503));
#1971=EDGE_LOOP('',(#6504,#6505,#6506,#6507,#6508,#6509,#6510));
#1972=EDGE_LOOP('',(#6511,#6512,#6513,#6514));
#1973=EDGE_LOOP('',(#6515));
#1974=EDGE_LOOP('',(#6516,#6517,#6518,#6519,#6520,#6521,#6522));
#1975=EDGE_LOOP('',(#6523,#6524,#6525,#6526));
#1976=EDGE_LOOP('',(#6527));
#1977=EDGE_LOOP('',(#6528));
#1978=EDGE_LOOP('',(#6529,#6530,#6531,#6532));
#1979=EDGE_LOOP('',(#6533,#6534));
#1980=EDGE_LOOP('',(#6535,#6536,#6537,#6538,#6539,#6540,#6541,#6542));
#1981=EDGE_LOOP('',(#6543,#6544,#6545));
#1982=EDGE_LOOP('',(#6546,#6547,#6548,#6549));
#1983=EDGE_LOOP('',(#6550));
#1984=EDGE_LOOP('',(#6551));
#1985=EDGE_LOOP('',(#6552,#6553,#6554,#6555));
#1986=EDGE_LOOP('',(#6556,#6557));
#1987=EDGE_LOOP('',(#6558));
#1988=EDGE_LOOP('',(#6559,#6560,#6561,#6562,#6563,#6564,#6565,#6566,#6567));
#1989=EDGE_LOOP('',(#6568));
#1990=EDGE_LOOP('',(#6569,#6570,#6571,#6572));
#1991=EDGE_LOOP('',(#6573,#6574,#6575,#6576));
#1992=EDGE_LOOP('',(#6577,#6578,#6579,#6580));
#1993=EDGE_LOOP('',(#6581,#6582,#6583,#6584));
#1994=EDGE_LOOP('',(#6585,#6586,#6587,#6588));
#1995=EDGE_LOOP('',(#6589));
#1996=EDGE_LOOP('',(#6590,#6591,#6592,#6593,#6594,#6595,#6596));
#1997=EDGE_LOOP('',(#6597,#6598,#6599,#6600));
#1998=EDGE_LOOP('',(#6601));
#1999=EDGE_LOOP('',(#6602,#6603,#6604,#6605,#6606,#6607,#6608));
#2000=EDGE_LOOP('',(#6609,#6610,#6611,#6612));
#2001=EDGE_LOOP('',(#6613));
#2002=EDGE_LOOP('',(#6614));
#2003=EDGE_LOOP('',(#6615,#6616,#6617,#6618));
#2004=EDGE_LOOP('',(#6619,#6620,#6621,#6622));
#2005=EDGE_LOOP('',(#6623,#6624,#6625,#6626));
#2006=EDGE_LOOP('',(#6627,#6628,#6629,#6630));
#2007=EDGE_LOOP('',(#6631,#6632,#6633,#6634));
#2008=EDGE_LOOP('',(#6635,#6636,#6637,#6638));
#2009=EDGE_LOOP('',(#6639,#6640,#6641,#6642,#6643,#6644));
#2010=EDGE_LOOP('',(#6645,#6646,#6647,#6648,#6649,#6650));
#2011=EDGE_LOOP('',(#6651));
#2012=EDGE_LOOP('',(#6652));
#2013=EDGE_LOOP('',(#6653,#6654,#6655,#6656));
#2014=EDGE_LOOP('',(#6657,#6658,#6659,#6660));
#2015=EDGE_LOOP('',(#6661,#6662,#6663,#6664));
#2016=EDGE_LOOP('',(#6665));
#2017=EDGE_LOOP('',(#6666));
#2018=EDGE_LOOP('',(#6667,#6668,#6669,#6670));
#2019=EDGE_LOOP('',(#6671,#6672,#6673,#6674));
#2020=EDGE_LOOP('',(#6675,#6676,#6677,#6678,#6679,#6680));
#2021=EDGE_LOOP('',(#6681,#6682,#6683,#6684,#6685));
#2022=EDGE_LOOP('',(#6686,#6687,#6688,#6689));
#2023=EDGE_LOOP('',(#6690,#6691,#6692,#6693));
#2024=EDGE_LOOP('',(#6694));
#2025=EDGE_LOOP('',(#6695));
#2026=EDGE_LOOP('',(#6696,#6697,#6698,#6699,#6700));
#2027=EDGE_LOOP('',(#6701));
#2028=EDGE_LOOP('',(#6702));
#2029=EDGE_LOOP('',(#6703,#6704,#6705,#6706));
#2030=EDGE_LOOP('',(#6707,#6708,#6709,#6710,#6711,#6712));
#2031=EDGE_LOOP('',(#6713,#6714,#6715,#6716,#6717));
#2032=EDGE_LOOP('',(#6718));
#2033=EDGE_LOOP('',(#6719));
#2034=EDGE_LOOP('',(#6720,#6721,#6722,#6723));
#2035=EDGE_LOOP('',(#6724,#6725,#6726,#6727));
#2036=EDGE_LOOP('',(#6728,#6729,#6730,#6731));
#2037=EDGE_LOOP('',(#6732));
#2038=EDGE_LOOP('',(#6733));
#2039=EDGE_LOOP('',(#6734,#6735,#6736,#6737,#6738));
#2040=EDGE_LOOP('',(#6739,#6740));
#2041=EDGE_LOOP('',(#6741,#6742));
#2042=EDGE_LOOP('',(#6743,#6744));
#2043=EDGE_LOOP('',(#6745,#6746));
#2044=EDGE_LOOP('',(#6747,#6748));
#2045=EDGE_LOOP('',(#6749,#6750));
#2046=EDGE_LOOP('',(#6751,#6752));
#2047=EDGE_LOOP('',(#6753,#6754));
#2048=EDGE_LOOP('',(#6755,#6756,#6757,#6758));
#2049=EDGE_LOOP('',(#6759,#6760,#6761,#6762,#6763,#6764,#6765,#6766,#6767,
#6768,#6769,#6770,#6771,#6772,#6773,#6774,#6775,#6776,#6777,#6778));
#2050=EDGE_LOOP('',(#6779,#6780,#6781,#6782));
#2051=EDGE_LOOP('',(#6783,#6784,#6785,#6786));
#2052=EDGE_LOOP('',(#6787,#6788,#6789,#6790));
#2053=EDGE_LOOP('',(#6791,#6792,#6793,#6794));
#2054=EDGE_LOOP('',(#6795,#6796,#6797,#6798));
#2055=EDGE_LOOP('',(#6799,#6800,#6801,#6802,#6803,#6804));
#2056=EDGE_LOOP('',(#6805,#6806,#6807,#6808));
#2057=EDGE_LOOP('',(#6809,#6810,#6811,#6812));
#2058=EDGE_LOOP('',(#6813,#6814,#6815,#6816));
#2059=EDGE_LOOP('',(#6817,#6818,#6819,#6820));
#2060=EDGE_LOOP('',(#6821,#6822,#6823,#6824));
#2061=EDGE_LOOP('',(#6825,#6826,#6827,#6828));
#2062=EDGE_LOOP('',(#6829,#6830,#6831,#6832,#6833,#6834,#6835,#6836,#6837,
#6838,#6839,#6840,#6841,#6842,#6843,#6844,#6845,#6846,#6847,#6848));
#2063=EDGE_LOOP('',(#6849,#6850,#6851,#6852));
#2064=EDGE_LOOP('',(#6853,#6854,#6855,#6856));
#2065=EDGE_LOOP('',(#6857));
#2066=EDGE_LOOP('',(#6858));
#2067=EDGE_LOOP('',(#6859,#6860,#6861,#6862));
#2068=EDGE_LOOP('',(#6863));
#2069=EDGE_LOOP('',(#6864));
#2070=EDGE_LOOP('',(#6865,#6866,#6867,#6868));
#2071=EDGE_LOOP('',(#6869));
#2072=EDGE_LOOP('',(#6870));
#2073=EDGE_LOOP('',(#6871,#6872,#6873,#6874));
#2074=EDGE_LOOP('',(#6875));
#2075=EDGE_LOOP('',(#6876));
#2076=EDGE_LOOP('',(#6877,#6878,#6879,#6880));
#2077=EDGE_LOOP('',(#6881));
#2078=EDGE_LOOP('',(#6882));
#2079=EDGE_LOOP('',(#6883,#6884,#6885,#6886));
#2080=EDGE_LOOP('',(#6887));
#2081=EDGE_LOOP('',(#6888,#6889,#6890,#6891));
#2082=EDGE_LOOP('',(#6892,#6893,#6894,#6895));
#2083=EDGE_LOOP('',(#6896));
#2084=EDGE_LOOP('',(#6897,#6898,#6899,#6900));
#2085=EDGE_LOOP('',(#6901,#6902,#6903,#6904));
#2086=EDGE_LOOP('',(#6905,#6906,#6907,#6908));
#2087=EDGE_LOOP('',(#6909,#6910,#6911,#6912));
#2088=EDGE_LOOP('',(#6913,#6914,#6915,#6916));
#2089=EDGE_LOOP('',(#6917,#6918,#6919,#6920));
#2090=EDGE_LOOP('',(#6921,#6922,#6923,#6924,#6925,#6926));
#2091=EDGE_LOOP('',(#6927));
#2092=EDGE_LOOP('',(#6928,#6929,#6930,#6931,#6932,#6933));
#2093=EDGE_LOOP('',(#6934,#6935,#6936,#6937));
#2094=EDGE_LOOP('',(#6938,#6939,#6940,#6941));
#2095=EDGE_LOOP('',(#6942,#6943,#6944,#6945));
#2096=EDGE_LOOP('',(#6946));
#2097=EDGE_LOOP('',(#6947,#6948,#6949,#6950));
#2098=EDGE_LOOP('',(#6951,#6952,#6953,#6954));
#2099=EDGE_LOOP('',(#6955,#6956,#6957,#6958));
#2100=EDGE_LOOP('',(#6959,#6960,#6961,#6962));
#2101=EDGE_LOOP('',(#6963,#6964,#6965,#6966));
#2102=EDGE_LOOP('',(#6967,#6968,#6969,#6970,#6971,#6972,#6973,#6974,#6975,
#6976,#6977,#6978));
#2103=EDGE_LOOP('',(#6979));
#2104=EDGE_LOOP('',(#6980));
#2105=EDGE_LOOP('',(#6981));
#2106=EDGE_LOOP('',(#6982,#6983,#6984,#6985));
#2107=EDGE_LOOP('',(#6986,#6987,#6988,#6989));
#2108=EDGE_LOOP('',(#6990,#6991,#6992,#6993));
#2109=EDGE_LOOP('',(#6994,#6995,#6996,#6997));
#2110=EDGE_LOOP('',(#6998,#6999,#7000,#7001));
#2111=EDGE_LOOP('',(#7002,#7003,#7004,#7005,#7006,#7007,#7008,#7009,#7010,
#7011,#7012,#7013));
#2112=EDGE_LOOP('',(#7014));
#2113=EDGE_LOOP('',(#7015));
#2114=EDGE_LOOP('',(#7016));
#2115=EDGE_LOOP('',(#7017));
#2116=EDGE_LOOP('',(#7018,#7019,#7020,#7021));
#2117=EDGE_LOOP('',(#7022,#7023,#7024,#7025));
#2118=EDGE_LOOP('',(#7026,#7027,#7028,#7029));
#2119=EDGE_LOOP('',(#7030,#7031,#7032,#7033));
#2120=EDGE_LOOP('',(#7034,#7035,#7036,#7037));
#2121=EDGE_LOOP('',(#7038));
#2122=EDGE_LOOP('',(#7039));
#2123=EDGE_LOOP('',(#7040,#7041,#7042,#7043));
#2124=EDGE_LOOP('',(#7044,#7045,#7046,#7047));
#2125=EDGE_LOOP('',(#7048));
#2126=EDGE_LOOP('',(#7049,#7050,#7051,#7052));
#2127=EDGE_LOOP('',(#7053));
#2128=EDGE_LOOP('',(#7054,#7055,#7056,#7057));
#2129=EDGE_LOOP('',(#7058));
#2130=EDGE_LOOP('',(#7059));
#2131=EDGE_LOOP('',(#7060));
#2132=EDGE_LOOP('',(#7061,#7062,#7063,#7064));
#2133=EDGE_LOOP('',(#7065,#7066,#7067,#7068));
#2134=EDGE_LOOP('',(#7069));
#2135=EDGE_LOOP('',(#7070));
#2136=EDGE_LOOP('',(#7071));
#2137=EDGE_LOOP('',(#7072));
#2138=EDGE_LOOP('',(#7073,#7074));
#2139=EDGE_LOOP('',(#7075,#7076,#7077,#7078,#7079,#7080,#7081,#7082,#7083));
#2140=EDGE_LOOP('',(#7084,#7085));
#2141=EDGE_LOOP('',(#7086,#7087,#7088,#7089));
#2142=EDGE_LOOP('',(#7090,#7091,#7092,#7093,#7094));
#2143=EDGE_LOOP('',(#7095,#7096,#7097,#7098));
#2144=EDGE_LOOP('',(#7099,#7100));
#2145=EDGE_LOOP('',(#7101));
#2146=EDGE_LOOP('',(#7102));
#2147=EDGE_LOOP('',(#7103));
#2148=EDGE_LOOP('',(#7104));
#2149=EDGE_LOOP('',(#7105,#7106,#7107,#7108));
#2150=EDGE_LOOP('',(#7109));
#2151=EDGE_LOOP('',(#7110));
#2152=EDGE_LOOP('',(#7111));
#2153=EDGE_LOOP('',(#7112));
#2154=EDGE_LOOP('',(#7113));
#2155=EDGE_LOOP('',(#7114,#7115,#7116,#7117));
#2156=EDGE_LOOP('',(#7118,#7119,#7120,#7121));
#2157=EDGE_LOOP('',(#7122,#7123,#7124,#7125));
#2158=EDGE_LOOP('',(#7126));
#2159=EDGE_LOOP('',(#7127));
#2160=EDGE_LOOP('',(#7128));
#2161=EDGE_LOOP('',(#7129,#7130,#7131,#7132));
#2162=EDGE_LOOP('',(#7133,#7134,#7135,#7136));
#2163=EDGE_LOOP('',(#7137));
#2164=EDGE_LOOP('',(#7138));
#2165=EDGE_LOOP('',(#7139));
#2166=EDGE_LOOP('',(#7140));
#2167=EDGE_LOOP('',(#7141,#7142,#7143,#7144));
#2168=EDGE_LOOP('',(#7145,#7146,#7147,#7148));
#2169=EDGE_LOOP('',(#7149));
#2170=EDGE_LOOP('',(#7150));
#2171=EDGE_LOOP('',(#7151));
#2172=EDGE_LOOP('',(#7152));
#2173=EDGE_LOOP('',(#7153,#7154,#7155,#7156));
#2174=EDGE_LOOP('',(#7157,#7158,#7159,#7160));
#2175=EDGE_LOOP('',(#7161));
#2176=EDGE_LOOP('',(#7162));
#2177=EDGE_LOOP('',(#7163));
#2178=EDGE_LOOP('',(#7164));
#2179=EDGE_LOOP('',(#7165,#7166,#7167,#7168));
#2180=EDGE_LOOP('',(#7169));
#2181=EDGE_LOOP('',(#7170));
#2182=EDGE_LOOP('',(#7171));
#2183=EDGE_LOOP('',(#7172));
#2184=EDGE_LOOP('',(#7173));
#2185=EDGE_LOOP('',(#7174,#7175,#7176,#7177));
#2186=EDGE_LOOP('',(#7178,#7179,#7180,#7181));
#2187=EDGE_LOOP('',(#7182,#7183,#7184,#7185));
#2188=EDGE_LOOP('',(#7186));
#2189=EDGE_LOOP('',(#7187));
#2190=EDGE_LOOP('',(#7188));
#2191=EDGE_LOOP('',(#7189,#7190,#7191,#7192));
#2192=EDGE_LOOP('',(#7193,#7194,#7195,#7196));
#2193=EDGE_LOOP('',(#7197));
#2194=EDGE_LOOP('',(#7198));
#2195=EDGE_LOOP('',(#7199));
#2196=EDGE_LOOP('',(#7200));
#2197=EDGE_LOOP('',(#7201,#7202,#7203,#7204));
#2198=EDGE_LOOP('',(#7205,#7206,#7207,#7208));
#2199=EDGE_LOOP('',(#7209));
#2200=EDGE_LOOP('',(#7210));
#2201=EDGE_LOOP('',(#7211));
#2202=EDGE_LOOP('',(#7212));
#2203=EDGE_LOOP('',(#7213,#7214,#7215,#7216));
#2204=EDGE_LOOP('',(#7217,#7218,#7219,#7220));
#2205=EDGE_LOOP('',(#7221));
#2206=EDGE_LOOP('',(#7222));
#2207=EDGE_LOOP('',(#7223));
#2208=EDGE_LOOP('',(#7224));
#2209=EDGE_LOOP('',(#7225));
#2210=EDGE_LOOP('',(#7226,#7227,#7228,#7229));
#2211=EDGE_LOOP('',(#7230,#7231,#7232,#7233));
#2212=EDGE_LOOP('',(#7234,#7235,#7236,#7237));
#2213=EDGE_LOOP('',(#7238));
#2214=EDGE_LOOP('',(#7239));
#2215=EDGE_LOOP('',(#7240,#7241,#7242,#7243));
#2216=EDGE_LOOP('',(#7244,#7245,#7246,#7247));
#2217=EDGE_LOOP('',(#7248,#7249,#7250,#7251));
#2218=EDGE_LOOP('',(#7252));
#2219=EDGE_LOOP('',(#7253,#7254,#7255,#7256));
#2220=EDGE_LOOP('',(#7257,#7258,#7259,#7260));
#2221=EDGE_LOOP('',(#7261,#7262,#7263,#7264));
#2222=EDGE_LOOP('',(#7265,#7266,#7267,#7268));
#2223=EDGE_LOOP('',(#7269,#7270,#7271,#7272));
#2224=EDGE_LOOP('',(#7273,#7274,#7275,#7276));
#2225=EDGE_LOOP('',(#7277,#7278,#7279,#7280,#7281,#7282));
#2226=EDGE_LOOP('',(#7283,#7284,#7285,#7286,#7287,#7288));
#2227=EDGE_LOOP('',(#7289));
#2228=EDGE_LOOP('',(#7290,#7291,#7292,#7293));
#2229=EDGE_LOOP('',(#7294,#7295,#7296,#7297));
#2230=EDGE_LOOP('',(#7298,#7299,#7300,#7301));
#2231=EDGE_LOOP('',(#7302,#7303,#7304,#7305));
#2232=EDGE_LOOP('',(#7306,#7307,#7308,#7309));
#2233=EDGE_LOOP('',(#7310,#7311,#7312,#7313));
#2234=EDGE_LOOP('',(#7314,#7315,#7316,#7317,#7318,#7319));
#2235=EDGE_LOOP('',(#7320));
#2236=EDGE_LOOP('',(#7321,#7322,#7323,#7324,#7325,#7326));
#2237=EDGE_LOOP('',(#7327,#7328,#7329,#7330));
#2238=EDGE_LOOP('',(#7331,#7332,#7333,#7334));
#2239=EDGE_LOOP('',(#7335,#7336,#7337,#7338));
#2240=EDGE_LOOP('',(#7339,#7340,#7341,#7342));
#2241=EDGE_LOOP('',(#7343,#7344,#7345,#7346));
#2242=EDGE_LOOP('',(#7347,#7348,#7349,#7350));
#2243=EDGE_LOOP('',(#7351,#7352,#7353,#7354));
#2244=EDGE_LOOP('',(#7355));
#2245=EDGE_LOOP('',(#7356));
#2246=EDGE_LOOP('',(#7357,#7358,#7359,#7360));
#2247=EDGE_LOOP('',(#7361,#7362,#7363,#7364));
#2248=EDGE_LOOP('',(#7365,#7366,#7367,#7368));
#2249=EDGE_LOOP('',(#7369));
#2250=EDGE_LOOP('',(#7370));
#2251=EDGE_LOOP('',(#7371,#7372,#7373,#7374));
#2252=EDGE_LOOP('',(#7375,#7376,#7377,#7378));
#2253=EDGE_LOOP('',(#7379));
#2254=EDGE_LOOP('',(#7380));
#2255=EDGE_LOOP('',(#7381));
#2256=EDGE_LOOP('',(#7382));
#2257=EDGE_LOOP('',(#7383,#7384,#7385,#7386));
#2258=EDGE_LOOP('',(#7387,#7388,#7389,#7390));
#2259=EDGE_LOOP('',(#7391));
#2260=EDGE_LOOP('',(#7392));
#2261=EDGE_LOOP('',(#7393));
#2262=EDGE_LOOP('',(#7394));
#2263=EDGE_LOOP('',(#7395,#7396,#7397,#7398));
#2264=EDGE_LOOP('',(#7399,#7400,#7401,#7402));
#2265=EDGE_LOOP('',(#7403,#7404,#7405,#7406));
#2266=EDGE_LOOP('',(#7407,#7408,#7409,#7410));
#2267=EDGE_LOOP('',(#7411,#7412,#7413,#7414));
#2268=EDGE_LOOP('',(#7415));
#2269=EDGE_LOOP('',(#7416));
#2270=EDGE_LOOP('',(#7417,#7418,#7419,#7420));
#2271=EDGE_LOOP('',(#7421,#7422,#7423,#7424));
#2272=EDGE_LOOP('',(#7425,#7426,#7427,#7428));
#2273=EDGE_LOOP('',(#7429));
#2274=EDGE_LOOP('',(#7430));
#2275=EDGE_LOOP('',(#7431,#7432,#7433,#7434));
#2276=EDGE_LOOP('',(#7435,#7436,#7437,#7438));
#2277=EDGE_LOOP('',(#7439));
#2278=EDGE_LOOP('',(#7440));
#2279=EDGE_LOOP('',(#7441));
#2280=EDGE_LOOP('',(#7442));
#2281=EDGE_LOOP('',(#7443,#7444,#7445,#7446));
#2282=EDGE_LOOP('',(#7447,#7448,#7449,#7450));
#2283=EDGE_LOOP('',(#7451));
#2284=EDGE_LOOP('',(#7452));
#2285=EDGE_LOOP('',(#7453));
#2286=EDGE_LOOP('',(#7454));
#2287=EDGE_LOOP('',(#7455,#7456,#7457,#7458));
#2288=EDGE_LOOP('',(#7459));
#2289=EDGE_LOOP('',(#7460,#7461,#7462,#7463));
#2290=EDGE_LOOP('',(#7464,#7465,#7466,#7467));
#2291=EDGE_LOOP('',(#7468,#7469,#7470,#7471));
#2292=EDGE_LOOP('',(#7472,#7473,#7474,#7475));
#2293=EDGE_LOOP('',(#7476,#7477,#7478,#7479));
#2294=EDGE_LOOP('',(#7480,#7481,#7482,#7483));
#2295=EDGE_LOOP('',(#7484,#7485,#7486,#7487));
#2296=EDGE_LOOP('',(#7488));
#2297=EDGE_LOOP('',(#7489));
#2298=EDGE_LOOP('',(#7490));
#2299=EDGE_LOOP('',(#7491));
#2300=EDGE_LOOP('',(#7492));
#2301=EDGE_LOOP('',(#7493,#7494,#7495,#7496));
#2302=EDGE_LOOP('',(#7497,#7498,#7499,#7500));
#2303=EDGE_LOOP('',(#7501));
#2304=EDGE_LOOP('',(#7502));
#2305=EDGE_LOOP('',(#7503));
#2306=EDGE_LOOP('',(#7504));
#2307=EDGE_LOOP('',(#7505));
#2308=EDGE_LOOP('',(#7506,#7507,#7508,#7509));
#2309=EDGE_LOOP('',(#7510));
#2310=EDGE_LOOP('',(#7511,#7512,#7513,#7514));
#2311=EDGE_LOOP('',(#7515,#7516,#7517,#7518));
#2312=EDGE_LOOP('',(#7519,#7520,#7521,#7522));
#2313=EDGE_LOOP('',(#7523,#7524,#7525,#7526));
#2314=EDGE_LOOP('',(#7527,#7528,#7529,#7530));
#2315=EDGE_LOOP('',(#7531,#7532,#7533,#7534));
#2316=EDGE_LOOP('',(#7535,#7536,#7537,#7538));
#2317=EDGE_LOOP('',(#7539,#7540,#7541,#7542));
#2318=EDGE_LOOP('',(#7543));
#2319=EDGE_LOOP('',(#7544));
#2320=EDGE_LOOP('',(#7545));
#2321=EDGE_LOOP('',(#7546));
#2322=EDGE_LOOP('',(#7547));
#2323=EDGE_LOOP('',(#7548,#7549,#7550,#7551));
#2324=EDGE_LOOP('',(#7552,#7553,#7554,#7555));
#2325=EDGE_LOOP('',(#7556));
#2326=EDGE_LOOP('',(#7557));
#2327=EDGE_LOOP('',(#7558));
#2328=EDGE_LOOP('',(#7559));
#2329=EDGE_LOOP('',(#7560));
#2330=EDGE_LOOP('',(#7561,#7562,#7563,#7564));
#2331=EDGE_LOOP('',(#7565,#7566,#7567,#7568));
#2332=EDGE_LOOP('',(#7569,#7570,#7571,#7572));
#2333=EDGE_LOOP('',(#7573,#7574,#7575,#7576));
#2334=EDGE_LOOP('',(#7577,#7578,#7579,#7580));
#2335=EDGE_LOOP('',(#7581,#7582,#7583,#7584));
#2336=EDGE_LOOP('',(#7585,#7586,#7587,#7588));
#2337=EDGE_LOOP('',(#7589,#7590,#7591,#7592));
#2338=EDGE_LOOP('',(#7593,#7594,#7595,#7596));
#2339=EDGE_LOOP('',(#7597));
#2340=EDGE_LOOP('',(#7598));
#2341=EDGE_LOOP('',(#7599));
#2342=EDGE_LOOP('',(#7600));
#2343=EDGE_LOOP('',(#7601));
#2344=EDGE_LOOP('',(#7602,#7603,#7604,#7605));
#2345=EDGE_LOOP('',(#7606,#7607,#7608,#7609));
#2346=EDGE_LOOP('',(#7610));
#2347=EDGE_LOOP('',(#7611));
#2348=EDGE_LOOP('',(#7612));
#2349=EDGE_LOOP('',(#7613));
#2350=EDGE_LOOP('',(#7614));
#2351=EDGE_LOOP('',(#7615,#7616,#7617,#7618));
#2352=EDGE_LOOP('',(#7619,#7620,#7621,#7622));
#2353=EDGE_LOOP('',(#7623,#7624,#7625,#7626));
#2354=EDGE_LOOP('',(#7627));
#2355=EDGE_LOOP('',(#7628));
#2356=EDGE_LOOP('',(#7629));
#2357=EDGE_LOOP('',(#7630));
#2358=EDGE_LOOP('',(#7631));
#2359=EDGE_LOOP('',(#7632,#7633,#7634,#7635));
#2360=EDGE_LOOP('',(#7636,#7637,#7638,#7639));
#2361=EDGE_LOOP('',(#7640,#7641,#7642,#7643));
#2362=EDGE_LOOP('',(#7644));
#2363=EDGE_LOOP('',(#7645));
#2364=EDGE_LOOP('',(#7646));
#2365=EDGE_LOOP('',(#7647,#7648,#7649,#7650));
#2366=EDGE_LOOP('',(#7651,#7652,#7653,#7654));
#2367=EDGE_LOOP('',(#7655));
#2368=EDGE_LOOP('',(#7656));
#2369=EDGE_LOOP('',(#7657));
#2370=EDGE_LOOP('',(#7658));
#2371=EDGE_LOOP('',(#7659,#7660,#7661,#7662));
#2372=EDGE_LOOP('',(#7663,#7664,#7665,#7666));
#2373=EDGE_LOOP('',(#7667));
#2374=EDGE_LOOP('',(#7668));
#2375=EDGE_LOOP('',(#7669));
#2376=EDGE_LOOP('',(#7670));
#2377=EDGE_LOOP('',(#7671,#7672,#7673,#7674));
#2378=EDGE_LOOP('',(#7675,#7676,#7677,#7678));
#2379=EDGE_LOOP('',(#7679));
#2380=EDGE_LOOP('',(#7680));
#2381=EDGE_LOOP('',(#7681));
#2382=EDGE_LOOP('',(#7682));
#2383=EDGE_LOOP('',(#7683,#7684,#7685,#7686));
#2384=EDGE_LOOP('',(#7687));
#2385=EDGE_LOOP('',(#7688,#7689,#7690,#7691));
#2386=EDGE_LOOP('',(#7692,#7693,#7694,#7695));
#2387=EDGE_LOOP('',(#7696,#7697,#7698,#7699));
#2388=EDGE_LOOP('',(#7700,#7701,#7702,#7703));
#2389=EDGE_LOOP('',(#7704,#7705,#7706,#7707));
#2390=EDGE_LOOP('',(#7708,#7709,#7710,#7711));
#2391=EDGE_LOOP('',(#7712));
#2392=EDGE_LOOP('',(#7713));
#2393=EDGE_LOOP('',(#7714));
#2394=EDGE_LOOP('',(#7715));
#2395=EDGE_LOOP('',(#7716));
#2396=EDGE_LOOP('',(#7717,#7718,#7719,#7720));
#2397=EDGE_LOOP('',(#7721,#7722,#7723,#7724));
#2398=EDGE_LOOP('',(#7725));
#2399=EDGE_LOOP('',(#7726));
#2400=EDGE_LOOP('',(#7727));
#2401=EDGE_LOOP('',(#7728));
#2402=EDGE_LOOP('',(#7729));
#2403=EDGE_LOOP('',(#7730,#7731,#7732,#7733));
#2404=EDGE_LOOP('',(#7734,#7735,#7736,#7737));
#2405=EDGE_LOOP('',(#7738));
#2406=EDGE_LOOP('',(#7739,#7740,#7741,#7742));
#2407=EDGE_LOOP('',(#7743,#7744,#7745,#7746));
#2408=EDGE_LOOP('',(#7747,#7748,#7749,#7750));
#2409=EDGE_LOOP('',(#7751,#7752,#7753,#7754));
#2410=EDGE_LOOP('',(#7755,#7756,#7757,#7758));
#2411=EDGE_LOOP('',(#7759,#7760,#7761,#7762));
#2412=EDGE_LOOP('',(#7763,#7764,#7765,#7766));
#2413=EDGE_LOOP('',(#7767));
#2414=EDGE_LOOP('',(#7768));
#2415=EDGE_LOOP('',(#7769));
#2416=EDGE_LOOP('',(#7770));
#2417=EDGE_LOOP('',(#7771));
#2418=EDGE_LOOP('',(#7772,#7773,#7774,#7775));
#2419=EDGE_LOOP('',(#7776,#7777,#7778,#7779));
#2420=EDGE_LOOP('',(#7780));
#2421=EDGE_LOOP('',(#7781));
#2422=EDGE_LOOP('',(#7782));
#2423=EDGE_LOOP('',(#7783));
#2424=EDGE_LOOP('',(#7784));
#2425=EDGE_LOOP('',(#7785,#7786,#7787,#7788));
#2426=EDGE_LOOP('',(#7789,#7790,#7791,#7792));
#2427=EDGE_LOOP('',(#7793,#7794,#7795,#7796));
#2428=EDGE_LOOP('',(#7797,#7798,#7799,#7800));
#2429=EDGE_LOOP('',(#7801,#7802,#7803,#7804));
#2430=EDGE_LOOP('',(#7805,#7806,#7807,#7808));
#2431=EDGE_LOOP('',(#7809,#7810,#7811,#7812));
#2432=EDGE_LOOP('',(#7813,#7814,#7815,#7816));
#2433=EDGE_LOOP('',(#7817,#7818,#7819,#7820));
#2434=EDGE_LOOP('',(#7821));
#2435=EDGE_LOOP('',(#7822));
#2436=EDGE_LOOP('',(#7823));
#2437=EDGE_LOOP('',(#7824));
#2438=EDGE_LOOP('',(#7825));
#2439=EDGE_LOOP('',(#7826,#7827,#7828,#7829));
#2440=EDGE_LOOP('',(#7830,#7831,#7832,#7833));
#2441=EDGE_LOOP('',(#7834));
#2442=EDGE_LOOP('',(#7835));
#2443=EDGE_LOOP('',(#7836));
#2444=EDGE_LOOP('',(#7837));
#2445=EDGE_LOOP('',(#7838));
#2446=EDGE_LOOP('',(#7839,#7840,#7841,#7842));
#2447=EDGE_LOOP('',(#7843,#7844,#7845,#7846));
#2448=EDGE_LOOP('',(#7847,#7848,#7849,#7850));
#2449=EDGE_LOOP('',(#7851,#7852,#7853,#7854));
#2450=EDGE_LOOP('',(#7855));
#2451=EDGE_LOOP('',(#7856));
#2452=EDGE_LOOP('',(#7857));
#2453=EDGE_LOOP('',(#7858));
#2454=EDGE_LOOP('',(#7859));
#2455=EDGE_LOOP('',(#7860,#7861,#7862,#7863));
#2456=EDGE_LOOP('',(#7864,#7865,#7866,#7867));
#2457=EDGE_LOOP('',(#7868,#7869,#7870,#7871));
#2458=EDGE_LOOP('',(#7872));
#2459=EDGE_LOOP('',(#7873));
#2460=EDGE_LOOP('',(#7874));
#2461=EDGE_LOOP('',(#7875,#7876,#7877,#7878));
#2462=EDGE_LOOP('',(#7879,#7880,#7881,#7882));
#2463=EDGE_LOOP('',(#7883));
#2464=EDGE_LOOP('',(#7884));
#2465=EDGE_LOOP('',(#7885));
#2466=EDGE_LOOP('',(#7886));
#2467=EDGE_LOOP('',(#7887,#7888,#7889,#7890));
#2468=EDGE_LOOP('',(#7891,#7892,#7893,#7894));
#2469=EDGE_LOOP('',(#7895));
#2470=EDGE_LOOP('',(#7896));
#2471=EDGE_LOOP('',(#7897));
#2472=EDGE_LOOP('',(#7898));
#2473=EDGE_LOOP('',(#7899,#7900,#7901,#7902));
#2474=EDGE_LOOP('',(#7903,#7904,#7905,#7906));
#2475=EDGE_LOOP('',(#7907));
#2476=EDGE_LOOP('',(#7908));
#2477=EDGE_LOOP('',(#7909));
#2478=EDGE_LOOP('',(#7910));
#2479=EDGE_LOOP('',(#7911,#7912,#7913,#7914));
#2480=EDGE_LOOP('',(#7915,#7916,#7917,#7918));
#2481=EDGE_LOOP('',(#7919,#7920,#7921,#7922));
#2482=EDGE_LOOP('',(#7923,#7924,#7925,#7926));
#2483=EDGE_LOOP('',(#7927,#7928,#7929,#7930));
#2484=EDGE_LOOP('',(#7931));
#2485=EDGE_LOOP('',(#7932));
#2486=EDGE_LOOP('',(#7933,#7934,#7935,#7936));
#2487=EDGE_LOOP('',(#7937));
#2488=EDGE_LOOP('',(#7938));
#2489=EDGE_LOOP('',(#7939,#7940,#7941,#7942));
#2490=EDGE_LOOP('',(#7943));
#2491=EDGE_LOOP('',(#7944));
#2492=EDGE_LOOP('',(#7945,#7946,#7947,#7948));
#2493=EDGE_LOOP('',(#7949));
#2494=EDGE_LOOP('',(#7950));
#2495=EDGE_LOOP('',(#7951,#7952,#7953,#7954));
#2496=EDGE_LOOP('',(#7955));
#2497=EDGE_LOOP('',(#7956));
#2498=EDGE_LOOP('',(#7957,#7958,#7959,#7960));
#2499=EDGE_LOOP('',(#7961));
#2500=EDGE_LOOP('',(#7962));
#2501=EDGE_LOOP('',(#7963,#7964,#7965,#7966));
#2502=EDGE_LOOP('',(#7967,#7968,#7969,#7970));
#2503=EDGE_LOOP('',(#7971,#7972,#7973,#7974));
#2504=EDGE_LOOP('',(#7975,#7976,#7977,#7978));
#2505=EDGE_LOOP('',(#7979,#7980,#7981,#7982));
#2506=EDGE_LOOP('',(#7983,#7984,#7985,#7986));
#2507=EDGE_LOOP('',(#7987));
#2508=EDGE_LOOP('',(#7988));
#2509=EDGE_LOOP('',(#7989,#7990,#7991,#7992));
#2510=EDGE_LOOP('',(#7993,#7994,#7995,#7996));
#2511=EDGE_LOOP('',(#7997));
#2512=EDGE_LOOP('',(#7998));
#2513=EDGE_LOOP('',(#7999,#8000,#8001,#8002));
#2514=EDGE_LOOP('',(#8003,#8004,#8005,#8006));
#2515=EDGE_LOOP('',(#8007,#8008,#8009,#8010));
#2516=EDGE_LOOP('',(#8011,#8012,#8013,#8014));
#2517=EDGE_LOOP('',(#8015,#8016,#8017,#8018));
#2518=EDGE_LOOP('',(#8019,#8020,#8021,#8022));
#2519=EDGE_LOOP('',(#8023,#8024,#8025,#8026));
#2520=EDGE_LOOP('',(#8027,#8028,#8029,#8030));
#2521=EDGE_LOOP('',(#8031,#8032,#8033,#8034,#8035,#8036));
#2522=EDGE_LOOP('',(#8037,#8038,#8039,#8040,#8041,#8042));
#2523=EDGE_LOOP('',(#8043));
#2524=EDGE_LOOP('',(#8044));
#2525=EDGE_LOOP('',(#8045,#8046,#8047,#8048));
#2526=EDGE_LOOP('',(#8049,#8050,#8051,#8052));
#2527=EDGE_LOOP('',(#8053,#8054,#8055,#8056));
#2528=EDGE_LOOP('',(#8057));
#2529=EDGE_LOOP('',(#8058));
#2530=EDGE_LOOP('',(#8059,#8060,#8061,#8062));
#2531=EDGE_LOOP('',(#8063,#8064,#8065,#8066));
#2532=LINE('',#13538,#3081);
#2533=LINE('',#13544,#3082);
#2534=LINE('',#13550,#3083);
#2535=LINE('',#13556,#3084);
#2536=LINE('',#13562,#3085);
#2537=LINE('',#13568,#3086);
#2538=LINE('',#13574,#3087);
#2539=LINE('',#13580,#3088);
#2540=LINE('',#13586,#3089);
#2541=LINE('',#13592,#3090);
#2542=LINE('',#13598,#3091);
#2543=LINE('',#13604,#3092);
#2544=LINE('',#13609,#3093);
#2545=LINE('',#13611,#3094);
#2546=LINE('',#13613,#3095);
#2547=LINE('',#13614,#3096);
#2548=LINE('',#13617,#3097);
#2549=LINE('',#13619,#3098);
#2550=LINE('',#13620,#3099);
#2551=LINE('',#13623,#3100);
#2552=LINE('',#13625,#3101);
#2553=LINE('',#13626,#3102);
#2554=LINE('',#13628,#3103);
#2555=LINE('',#13629,#3104);
#2556=LINE('',#13636,#3105);
#2557=LINE('',#13638,#3106);
#2558=LINE('',#13640,#3107);
#2559=LINE('',#13641,#3108);
#2560=LINE('',#13644,#3109);
#2561=LINE('',#13646,#3110);
#2562=LINE('',#13647,#3111);
#2563=LINE('',#13650,#3112);
#2564=LINE('',#13652,#3113);
#2565=LINE('',#13653,#3114);
#2566=LINE('',#13655,#3115);
#2567=LINE('',#13656,#3116);
#2568=LINE('',#13663,#3117);
#2569=LINE('',#13665,#3118);
#2570=LINE('',#13667,#3119);
#2571=LINE('',#13668,#3120);
#2572=LINE('',#13671,#3121);
#2573=LINE('',#13673,#3122);
#2574=LINE('',#13674,#3123);
#2575=LINE('',#13677,#3124);
#2576=LINE('',#13679,#3125);
#2577=LINE('',#13680,#3126);
#2578=LINE('',#13682,#3127);
#2579=LINE('',#13683,#3128);
#2580=LINE('',#13727,#3129);
#2581=LINE('',#13769,#3130);
#2582=LINE('',#13776,#3131);
#2583=LINE('',#13783,#3132);
#2584=LINE('',#13790,#3133);
#2585=LINE('',#13800,#3134);
#2586=LINE('',#13803,#3135);
#2587=LINE('',#13807,#3136);
#2588=LINE('',#13811,#3137);
#2589=LINE('',#13818,#3138);
#2590=LINE('',#13822,#3139);
#2591=LINE('',#13829,#3140);
#2592=LINE('',#13833,#3141);
#2593=LINE('',#13841,#3142);
#2594=LINE('',#13861,#3143);
#2595=LINE('',#13865,#3144);
#2596=LINE('',#13869,#3145);
#2597=LINE('',#13873,#3146);
#2598=LINE('',#13878,#3147);
#2599=LINE('',#13885,#3148);
#2600=LINE('',#13889,#3149);
#2601=LINE('',#13898,#3150);
#2602=LINE('',#13907,#3151);
#2603=LINE('',#13916,#3152);
#2604=LINE('',#13925,#3153);
#2605=LINE('',#13933,#3154);
#2606=LINE('',#13937,#3155);
#2607=LINE('',#13941,#3156);
#2608=LINE('',#13945,#3157);
#2609=LINE('',#13950,#3158);
#2610=LINE('',#13958,#3159);
#2611=LINE('',#13963,#3160);
#2612=LINE('',#13971,#3161);
#2613=LINE('',#13975,#3162);
#2614=LINE('',#13980,#3163);
#2615=LINE('',#13984,#3164);
#2616=LINE('',#13989,#3165);
#2617=LINE('',#14022,#3166);
#2618=LINE('',#14025,#3167);
#2619=LINE('',#14028,#3168);
#2620=LINE('',#14035,#3169);
#2621=LINE('',#14043,#3170);
#2622=LINE('',#14044,#3171);
#2623=LINE('',#14046,#3172);
#2624=LINE('',#14048,#3173);
#2625=LINE('',#14049,#3174);
#2626=LINE('',#14050,#3175);
#2627=LINE('',#14054,#3176);
#2628=LINE('',#14058,#3177);
#2629=LINE('',#14062,#3178);
#2630=LINE('',#14064,#3179);
#2631=LINE('',#14069,#3180);
#2632=LINE('',#14070,#3181);
#2633=LINE('',#14071,#3182);
#2634=LINE('',#14074,#3183);
#2635=LINE('',#14075,#3184);
#2636=LINE('',#14078,#3185);
#2637=LINE('',#14079,#3186);
#2638=LINE('',#14081,#3187);
#2639=LINE('',#14087,#3188);
#2640=LINE('',#14091,#3189);
#2641=LINE('',#14096,#3190);
#2642=LINE('',#14100,#3191);
#2643=LINE('',#14105,#3192);
#2644=LINE('',#14138,#3193);
#2645=LINE('',#14141,#3194);
#2646=LINE('',#14144,#3195);
#2647=LINE('',#14151,#3196);
#2648=LINE('',#14159,#3197);
#2649=LINE('',#14160,#3198);
#2650=LINE('',#14162,#3199);
#2651=LINE('',#14164,#3200);
#2652=LINE('',#14165,#3201);
#2653=LINE('',#14166,#3202);
#2654=LINE('',#14170,#3203);
#2655=LINE('',#14174,#3204);
#2656=LINE('',#14178,#3205);
#2657=LINE('',#14180,#3206);
#2658=LINE('',#14185,#3207);
#2659=LINE('',#14186,#3208);
#2660=LINE('',#14187,#3209);
#2661=LINE('',#14190,#3210);
#2662=LINE('',#14191,#3211);
#2663=LINE('',#14194,#3212);
#2664=LINE('',#14195,#3213);
#2665=LINE('',#14197,#3214);
#2666=LINE('',#14203,#3215);
#2667=LINE('',#14207,#3216);
#2668=LINE('',#14212,#3217);
#2669=LINE('',#14229,#3218);
#2670=LINE('',#14244,#3219);
#2671=LINE('',#14249,#3220);
#2672=LINE('',#14251,#3221);
#2673=LINE('',#14257,#3222);
#2674=LINE('',#14264,#3223);
#2675=LINE('',#14266,#3224);
#2676=LINE('',#14268,#3225);
#2677=LINE('',#14269,#3226);
#2678=LINE('',#14271,#3227);
#2679=LINE('',#14272,#3228);
#2680=LINE('',#14276,#3229);
#2681=LINE('',#14280,#3230);
#2682=LINE('',#14285,#3231);
#2683=LINE('',#14290,#3232);
#2684=LINE('',#14291,#3233);
#2685=LINE('',#14292,#3234);
#2686=LINE('',#14295,#3235);
#2687=LINE('',#14296,#3236);
#2688=LINE('',#14299,#3237);
#2689=LINE('',#14300,#3238);
#2690=LINE('',#14302,#3239);
#2691=LINE('',#14308,#3240);
#2692=LINE('',#14312,#3241);
#2693=LINE('',#14317,#3242);
#2694=LINE('',#14334,#3243);
#2695=LINE('',#14349,#3244);
#2696=LINE('',#14354,#3245);
#2697=LINE('',#14356,#3246);
#2698=LINE('',#14362,#3247);
#2699=LINE('',#14369,#3248);
#2700=LINE('',#14371,#3249);
#2701=LINE('',#14373,#3250);
#2702=LINE('',#14374,#3251);
#2703=LINE('',#14376,#3252);
#2704=LINE('',#14377,#3253);
#2705=LINE('',#14381,#3254);
#2706=LINE('',#14385,#3255);
#2707=LINE('',#14390,#3256);
#2708=LINE('',#14395,#3257);
#2709=LINE('',#14396,#3258);
#2710=LINE('',#14397,#3259);
#2711=LINE('',#14400,#3260);
#2712=LINE('',#14401,#3261);
#2713=LINE('',#14404,#3262);
#2714=LINE('',#14405,#3263);
#2715=LINE('',#14407,#3264);
#2716=LINE('',#14413,#3265);
#2717=LINE('',#14415,#3266);
#2718=LINE('',#14417,#3267);
#2719=LINE('',#14418,#3268);
#2720=LINE('',#14421,#3269);
#2721=LINE('',#14423,#3270);
#2722=LINE('',#14424,#3271);
#2723=LINE('',#14427,#3272);
#2724=LINE('',#14429,#3273);
#2725=LINE('',#14430,#3274);
#2726=LINE('',#14433,#3275);
#2727=LINE('',#14435,#3276);
#2728=LINE('',#14436,#3277);
#2729=LINE('',#14439,#3278);
#2730=LINE('',#14441,#3279);
#2731=LINE('',#14442,#3280);
#2732=LINE('',#14444,#3281);
#2733=LINE('',#14445,#3282);
#2734=LINE('',#14457,#3283);
#2735=LINE('',#14461,#3284);
#2736=LINE('',#14465,#3285);
#2737=LINE('',#14472,#3286);
#2738=LINE('',#14474,#3287);
#2739=LINE('',#14489,#3288);
#2740=LINE('',#14495,#3289);
#2741=LINE('',#14499,#3290);
#2742=LINE('',#14505,#3291);
#2743=LINE('',#14510,#3292);
#2744=LINE('',#14525,#3293);
#2745=LINE('',#14534,#3294);
#2746=LINE('',#14538,#3295);
#2747=LINE('',#14542,#3296);
#2748=LINE('',#14545,#3297);
#2749=LINE('',#14698,#3298);
#2750=LINE('',#14994,#3299);
#2751=LINE('',#15036,#3300);
#2752=LINE('',#15041,#3301);
#2753=LINE('',#15050,#3302);
#2754=LINE('',#15055,#3303);
#2755=LINE('',#15069,#3304);
#2756=LINE('',#15072,#3305);
#2757=LINE('',#15078,#3306);
#2758=LINE('',#15080,#3307);
#2759=LINE('',#15082,#3308);
#2760=LINE('',#15083,#3309);
#2761=LINE('',#15086,#3310);
#2762=LINE('',#15088,#3311);
#2763=LINE('',#15089,#3312);
#2764=LINE('',#15092,#3313);
#2765=LINE('',#15094,#3314);
#2766=LINE('',#15095,#3315);
#2767=LINE('',#15098,#3316);
#2768=LINE('',#15100,#3317);
#2769=LINE('',#15101,#3318);
#2770=LINE('',#15104,#3319);
#2771=LINE('',#15106,#3320);
#2772=LINE('',#15107,#3321);
#2773=LINE('',#15109,#3322);
#2774=LINE('',#15110,#3323);
#2775=LINE('',#15118,#3324);
#2776=LINE('',#15122,#3325);
#2777=LINE('',#15126,#3326);
#2778=LINE('',#15134,#3327);
#2779=LINE('',#15140,#3328);
#2780=LINE('',#15146,#3329);
#2781=LINE('',#15151,#3330);
#2782=LINE('',#15155,#3331);
#2783=LINE('',#15159,#3332);
#2784=LINE('',#15161,#3333);
#2785=LINE('',#15162,#3334);
#2786=LINE('',#15165,#3335);
#2787=LINE('',#15169,#3336);
#2788=LINE('',#15173,#3337);
#2789=LINE('',#15177,#3338);
#2790=LINE('',#15181,#3339);
#2791=LINE('',#15185,#3340);
#2792=LINE('',#15186,#3341);
#2793=LINE('',#15189,#3342);
#2794=LINE('',#15194,#3343);
#2795=LINE('',#15197,#3344);
#2796=LINE('',#15199,#3345);
#2797=LINE('',#15203,#3346);
#2798=LINE('',#15204,#3347);
#2799=LINE('',#15207,#3348);
#2800=LINE('',#15211,#3349);
#2801=LINE('',#15213,#3350);
#2802=LINE('',#15218,#3351);
#2803=LINE('',#15219,#3352);
#2804=LINE('',#15221,#3353);
#2805=LINE('',#15230,#3354);
#2806=LINE('',#15233,#3355);
#2807=LINE('',#15241,#3356);
#2808=LINE('',#15248,#3357);
#2809=LINE('',#15257,#3358);
#2810=LINE('',#15263,#3359);
#2811=LINE('',#15271,#3360);
#2812=LINE('',#15301,#3361);
#2813=LINE('',#15348,#3362);
#2814=LINE('',#15353,#3363);
#2815=LINE('',#15359,#3364);
#2816=LINE('',#15368,#3365);
#2817=LINE('',#15382,#3366);
#2818=LINE('',#15385,#3367);
#2819=LINE('',#15390,#3368);
#2820=LINE('',#15398,#3369);
#2821=LINE('',#15404,#3370);
#2822=LINE('',#15413,#3371);
#2823=LINE('',#15419,#3372);
#2824=LINE('',#15428,#3373);
#2825=LINE('',#15434,#3374);
#2826=LINE('',#15443,#3375);
#2827=LINE('',#15457,#3376);
#2828=LINE('',#15460,#3377);
#2829=LINE('',#15465,#3378);
#2830=LINE('',#15473,#3379);
#2831=LINE('',#15479,#3380);
#2832=LINE('',#15488,#3381);
#2833=LINE('',#15494,#3382);
#2834=LINE('',#15503,#3383);
#2835=LINE('',#15509,#3384);
#2836=LINE('',#15520,#3385);
#2837=LINE('',#15524,#3386);
#2838=LINE('',#15528,#3387);
#2839=LINE('',#15535,#3388);
#2840=LINE('',#15539,#3389);
#2841=LINE('',#15543,#3390);
#2842=LINE('',#15548,#3391);
#2843=LINE('',#15550,#3392);
#2844=LINE('',#15552,#3393);
#2845=LINE('',#15553,#3394);
#2846=LINE('',#15556,#3395);
#2847=LINE('',#15558,#3396);
#2848=LINE('',#15559,#3397);
#2849=LINE('',#15562,#3398);
#2850=LINE('',#15564,#3399);
#2851=LINE('',#15565,#3400);
#2852=LINE('',#15568,#3401);
#2853=LINE('',#15570,#3402);
#2854=LINE('',#15571,#3403);
#2855=LINE('',#15574,#3404);
#2856=LINE('',#15576,#3405);
#2857=LINE('',#15577,#3406);
#2858=LINE('',#15579,#3407);
#2859=LINE('',#15580,#3408);
#2860=LINE('',#15590,#3409);
#2861=LINE('',#15592,#3410);
#2862=LINE('',#15594,#3411);
#2863=LINE('',#15595,#3412);
#2864=LINE('',#15598,#3413);
#2865=LINE('',#15600,#3414);
#2866=LINE('',#15601,#3415);
#2867=LINE('',#15604,#3416);
#2868=LINE('',#15606,#3417);
#2869=LINE('',#15607,#3418);
#2870=LINE('',#15610,#3419);
#2871=LINE('',#15612,#3420);
#2872=LINE('',#15613,#3421);
#2873=LINE('',#15616,#3422);
#2874=LINE('',#15618,#3423);
#2875=LINE('',#15619,#3424);
#2876=LINE('',#15621,#3425);
#2877=LINE('',#15622,#3426);
#2878=LINE('',#15630,#3427);
#2879=LINE('',#15632,#3428);
#2880=LINE('',#15639,#3429);
#2881=LINE('',#15645,#3430);
#2882=LINE('',#15650,#3431);
#2883=LINE('',#15654,#3432);
#2884=LINE('',#15658,#3433);
#2885=LINE('',#15660,#3434);
#2886=LINE('',#15661,#3435);
#2887=LINE('',#15664,#3436);
#2888=LINE('',#15668,#3437);
#2889=LINE('',#15669,#3438);
#2890=LINE('',#15678,#3439);
#2891=LINE('',#15684,#3440);
#2892=LINE('',#15693,#3441);
#2893=LINE('',#15699,#3442);
#2894=LINE('',#15712,#3443);
#2895=LINE('',#15718,#3444);
#2896=LINE('',#15723,#3445);
#2897=LINE('',#15727,#3446);
#2898=LINE('',#15731,#3447);
#2899=LINE('',#15733,#3448);
#2900=LINE('',#15734,#3449);
#2901=LINE('',#15737,#3450);
#2902=LINE('',#15741,#3451);
#2903=LINE('',#15742,#3452);
#2904=LINE('',#15751,#3453);
#2905=LINE('',#15757,#3454);
#2906=LINE('',#15766,#3455);
#2907=LINE('',#15772,#3456);
#2908=LINE('',#15785,#3457);
#2909=LINE('',#15792,#3458);
#2910=LINE('',#15798,#3459);
#2911=LINE('',#15804,#3460);
#2912=LINE('',#15810,#3461);
#2913=LINE('',#15816,#3462);
#2914=LINE('',#15821,#3463);
#2915=LINE('',#15823,#3464);
#2916=LINE('',#15825,#3465);
#2917=LINE('',#15826,#3466);
#2918=LINE('',#15829,#3467);
#2919=LINE('',#15831,#3468);
#2920=LINE('',#15832,#3469);
#2921=LINE('',#15835,#3470);
#2922=LINE('',#15837,#3471);
#2923=LINE('',#15838,#3472);
#2924=LINE('',#15840,#3473);
#2925=LINE('',#15841,#3474);
#2926=LINE('',#15849,#3475);
#2927=LINE('',#15855,#3476);
#2928=LINE('',#15861,#3477);
#2929=LINE('',#15867,#3478);
#2930=LINE('',#15873,#3479);
#2931=LINE('',#15878,#3480);
#2932=LINE('',#15880,#3481);
#2933=LINE('',#15882,#3482);
#2934=LINE('',#15883,#3483);
#2935=LINE('',#15886,#3484);
#2936=LINE('',#15888,#3485);
#2937=LINE('',#15889,#3486);
#2938=LINE('',#15892,#3487);
#2939=LINE('',#15894,#3488);
#2940=LINE('',#15895,#3489);
#2941=LINE('',#15897,#3490);
#2942=LINE('',#15898,#3491);
#2943=LINE('',#15906,#3492);
#2944=LINE('',#15912,#3493);
#2945=LINE('',#15918,#3494);
#2946=LINE('',#15924,#3495);
#2947=LINE('',#15930,#3496);
#2948=LINE('',#15935,#3497);
#2949=LINE('',#15937,#3498);
#2950=LINE('',#15939,#3499);
#2951=LINE('',#15940,#3500);
#2952=LINE('',#15943,#3501);
#2953=LINE('',#15945,#3502);
#2954=LINE('',#15946,#3503);
#2955=LINE('',#15949,#3504);
#2956=LINE('',#15951,#3505);
#2957=LINE('',#15952,#3506);
#2958=LINE('',#15954,#3507);
#2959=LINE('',#15955,#3508);
#2960=LINE('',#15963,#3509);
#2961=LINE('',#15977,#3510);
#2962=LINE('',#15980,#3511);
#2963=LINE('',#15985,#3512);
#2964=LINE('',#15993,#3513);
#2965=LINE('',#15999,#3514);
#2966=LINE('',#16008,#3515);
#2967=LINE('',#16014,#3516);
#2968=LINE('',#16023,#3517);
#2969=LINE('',#16029,#3518);
#2970=LINE('',#16039,#3519);
#2971=LINE('',#16046,#3520);
#2972=LINE('',#16052,#3521);
#2973=LINE('',#16058,#3522);
#2974=LINE('',#16064,#3523);
#2975=LINE('',#16070,#3524);
#2976=LINE('',#16075,#3525);
#2977=LINE('',#16077,#3526);
#2978=LINE('',#16079,#3527);
#2979=LINE('',#16080,#3528);
#2980=LINE('',#16083,#3529);
#2981=LINE('',#16085,#3530);
#2982=LINE('',#16086,#3531);
#2983=LINE('',#16089,#3532);
#2984=LINE('',#16091,#3533);
#2985=LINE('',#16092,#3534);
#2986=LINE('',#16094,#3535);
#2987=LINE('',#16095,#3536);
#2988=LINE('',#16103,#3537);
#2989=LINE('',#16109,#3538);
#2990=LINE('',#16115,#3539);
#2991=LINE('',#16121,#3540);
#2992=LINE('',#16127,#3541);
#2993=LINE('',#16132,#3542);
#2994=LINE('',#16134,#3543);
#2995=LINE('',#16136,#3544);
#2996=LINE('',#16137,#3545);
#2997=LINE('',#16140,#3546);
#2998=LINE('',#16142,#3547);
#2999=LINE('',#16143,#3548);
#3000=LINE('',#16146,#3549);
#3001=LINE('',#16148,#3550);
#3002=LINE('',#16149,#3551);
#3003=LINE('',#16151,#3552);
#3004=LINE('',#16152,#3553);
#3005=LINE('',#16160,#3554);
#3006=LINE('',#16166,#3555);
#3007=LINE('',#16172,#3556);
#3008=LINE('',#16178,#3557);
#3009=LINE('',#16184,#3558);
#3010=LINE('',#16189,#3559);
#3011=LINE('',#16191,#3560);
#3012=LINE('',#16193,#3561);
#3013=LINE('',#16194,#3562);
#3014=LINE('',#16197,#3563);
#3015=LINE('',#16199,#3564);
#3016=LINE('',#16200,#3565);
#3017=LINE('',#16203,#3566);
#3018=LINE('',#16205,#3567);
#3019=LINE('',#16206,#3568);
#3020=LINE('',#16208,#3569);
#3021=LINE('',#16209,#3570);
#3022=LINE('',#16217,#3571);
#3023=LINE('',#16231,#3572);
#3024=LINE('',#16234,#3573);
#3025=LINE('',#16239,#3574);
#3026=LINE('',#16247,#3575);
#3027=LINE('',#16253,#3576);
#3028=LINE('',#16262,#3577);
#3029=LINE('',#16268,#3578);
#3030=LINE('',#16277,#3579);
#3031=LINE('',#16283,#3580);
#3032=LINE('',#16294,#3581);
#3033=LINE('',#16296,#3582);
#3034=LINE('',#16297,#3583);
#3035=LINE('',#16300,#3584);
#3036=LINE('',#16302,#3585);
#3037=LINE('',#16303,#3586);
#3038=LINE('',#16308,#3587);
#3039=LINE('',#16309,#3588);
#3040=LINE('',#16311,#3589);
#3041=LINE('',#16312,#3590);
#3042=LINE('',#16322,#3591);
#3043=LINE('',#16329,#3592);
#3044=LINE('',#16336,#3593);
#3045=LINE('',#16343,#3594);
#3046=LINE('',#16350,#3595);
#3047=LINE('',#16355,#3596);
#3048=LINE('',#16362,#3597);
#3049=LINE('',#16365,#3598);
#3050=LINE('',#16368,#3599);
#3051=LINE('',#16370,#3600);
#3052=LINE('',#16371,#3601);
#3053=LINE('',#16377,#3602);
#3054=LINE('',#16379,#3603);
#3055=LINE('',#16380,#3604);
#3056=LINE('',#16389,#3605);
#3057=LINE('',#16394,#3606);
#3058=LINE('',#16401,#3607);
#3059=LINE('',#16403,#3608);
#3060=LINE('',#16405,#3609);
#3061=LINE('',#16406,#3610);
#3062=LINE('',#16409,#3611);
#3063=LINE('',#16411,#3612);
#3064=LINE('',#16412,#3613);
#3065=LINE('',#16415,#3614);
#3066=LINE('',#16417,#3615);
#3067=LINE('',#16418,#3616);
#3068=LINE('',#16421,#3617);
#3069=LINE('',#16423,#3618);
#3070=LINE('',#16424,#3619);
#3071=LINE('',#16427,#3620);
#3072=LINE('',#16429,#3621);
#3073=LINE('',#16430,#3622);
#3074=LINE('',#16432,#3623);
#3075=LINE('',#16433,#3624);
#3076=LINE('',#16445,#3625);
#3077=LINE('',#16449,#3626);
#3078=LINE('',#16453,#3627);
#3079=LINE('',#16460,#3628);
#3080=LINE('',#16462,#3629);
#3081=VECTOR('',#10640,0.165);
#3082=VECTOR('',#10647,0.165);
#3083=VECTOR('',#10654,0.165);
#3084=VECTOR('',#10661,0.165);
#3085=VECTOR('',#10668,0.164999999999999);
#3086=VECTOR('',#10675,0.164999999999999);
#3087=VECTOR('',#10682,0.165);
#3088=VECTOR('',#10689,0.165);
#3089=VECTOR('',#10696,0.21);
#3090=VECTOR('',#10703,0.21);
#3091=VECTOR('',#10710,0.21);
#3092=VECTOR('',#10717,0.21);
#3093=VECTOR('',#10722,1.);
#3094=VECTOR('',#10723,1.);
#3095=VECTOR('',#10724,1.);
#3096=VECTOR('',#10725,1.);
#3097=VECTOR('',#10728,1.);
#3098=VECTOR('',#10729,1.);
#3099=VECTOR('',#10730,1.);
#3100=VECTOR('',#10733,1.);
#3101=VECTOR('',#10734,1.);
#3102=VECTOR('',#10735,1.);
#3103=VECTOR('',#10738,1.);
#3104=VECTOR('',#10739,1.);
#3105=VECTOR('',#10748,1.);
#3106=VECTOR('',#10749,1.);
#3107=VECTOR('',#10750,1.);
#3108=VECTOR('',#10751,1.);
#3109=VECTOR('',#10754,1.);
#3110=VECTOR('',#10755,1.);
#3111=VECTOR('',#10756,1.);
#3112=VECTOR('',#10759,1.);
#3113=VECTOR('',#10760,1.);
#3114=VECTOR('',#10761,1.);
#3115=VECTOR('',#10764,1.);
#3116=VECTOR('',#10765,1.);
#3117=VECTOR('',#10774,1.);
#3118=VECTOR('',#10775,1.);
#3119=VECTOR('',#10776,1.);
#3120=VECTOR('',#10777,1.);
#3121=VECTOR('',#10780,1.);
#3122=VECTOR('',#10781,1.);
#3123=VECTOR('',#10782,1.);
#3124=VECTOR('',#10785,1.);
#3125=VECTOR('',#10786,1.);
#3126=VECTOR('',#10787,1.);
#3127=VECTOR('',#10790,1.);
#3128=VECTOR('',#10791,1.);
#3129=VECTOR('',#10800,0.25);
#3130=VECTOR('',#10805,0.165);
#3131=VECTOR('',#10814,0.165);
#3132=VECTOR('',#10823,0.165);
#3133=VECTOR('',#10832,0.165);
#3134=VECTOR('',#10845,1.);
#3135=VECTOR('',#10848,1.);
#3136=VECTOR('',#10851,1.);
#3137=VECTOR('',#10854,1.);
#3138=VECTOR('',#10863,1.);
#3139=VECTOR('',#10866,1.);
#3140=VECTOR('',#10875,1.);
#3141=VECTOR('',#10878,1.);
#3142=VECTOR('',#10889,2.2);
#3143=VECTOR('',#10916,0.275);
#3144=VECTOR('',#10921,0.275);
#3145=VECTOR('',#10926,0.275);
#3146=VECTOR('',#10931,0.275);
#3147=VECTOR('',#10936,1.5);
#3148=VECTOR('',#10945,3.);
#3149=VECTOR('',#10950,1.02);
#3150=VECTOR('',#10963,0.375);
#3151=VECTOR('',#10974,0.375);
#3152=VECTOR('',#10985,0.375);
#3153=VECTOR('',#10996,0.375);
#3154=VECTOR('',#11007,0.225);
#3155=VECTOR('',#11012,0.225);
#3156=VECTOR('',#11017,0.225);
#3157=VECTOR('',#11022,0.225);
#3158=VECTOR('',#11027,1.49);
#3159=VECTOR('',#11038,0.71);
#3160=VECTOR('',#11043,2.2);
#3161=VECTOR('',#11054,0.4);
#3162=VECTOR('',#11057,1.);
#3163=VECTOR('',#11062,0.4);
#3164=VECTOR('',#11065,1.);
#3165=VECTOR('',#11070,1.);
#3166=VECTOR('',#11077,0.165);
#3167=VECTOR('',#11082,1.);
#3168=VECTOR('',#11087,1.);
#3169=VECTOR('',#11098,1.);
#3170=VECTOR('',#11107,1.);
#3171=VECTOR('',#11108,1.);
#3172=VECTOR('',#11109,1.);
#3173=VECTOR('',#11110,1.);
#3174=VECTOR('',#11111,1.);
#3175=VECTOR('',#11112,1.);
#3176=VECTOR('',#11117,0.225);
#3177=VECTOR('',#11122,0.225);
#3178=VECTOR('',#11127,0.6);
#3179=VECTOR('',#11128,0.6);
#3180=VECTOR('',#11133,1.);
#3181=VECTOR('',#11134,1.);
#3182=VECTOR('',#11135,1.);
#3183=VECTOR('',#11138,1.);
#3184=VECTOR('',#11139,1.);
#3185=VECTOR('',#11142,1.);
#3186=VECTOR('',#11143,1.);
#3187=VECTOR('',#11146,1.);
#3188=VECTOR('',#11153,0.4);
#3189=VECTOR('',#11156,1.);
#3190=VECTOR('',#11161,0.4);
#3191=VECTOR('',#11164,1.);
#3192=VECTOR('',#11169,1.);
#3193=VECTOR('',#11176,0.164999999999999);
#3194=VECTOR('',#11181,1.);
#3195=VECTOR('',#11186,1.);
#3196=VECTOR('',#11197,1.);
#3197=VECTOR('',#11206,1.);
#3198=VECTOR('',#11207,1.);
#3199=VECTOR('',#11208,1.);
#3200=VECTOR('',#11209,1.);
#3201=VECTOR('',#11210,1.);
#3202=VECTOR('',#11211,1.);
#3203=VECTOR('',#11216,0.225);
#3204=VECTOR('',#11221,0.225);
#3205=VECTOR('',#11226,0.6);
#3206=VECTOR('',#11227,0.6);
#3207=VECTOR('',#11232,1.);
#3208=VECTOR('',#11233,1.);
#3209=VECTOR('',#11234,1.);
#3210=VECTOR('',#11237,1.);
#3211=VECTOR('',#11238,1.);
#3212=VECTOR('',#11241,1.);
#3213=VECTOR('',#11242,1.);
#3214=VECTOR('',#11245,1.);
#3215=VECTOR('',#11252,0.4);
#3216=VECTOR('',#11255,1.);
#3217=VECTOR('',#11260,1.);
#3218=VECTOR('',#11267,0.165);
#3219=VECTOR('',#11274,1.);
#3220=VECTOR('',#11279,1.);
#3221=VECTOR('',#11282,1.);
#3222=VECTOR('',#11291,1.);
#3223=VECTOR('',#11300,1.);
#3224=VECTOR('',#11301,1.);
#3225=VECTOR('',#11302,1.);
#3226=VECTOR('',#11303,1.);
#3227=VECTOR('',#11304,1.);
#3228=VECTOR('',#11305,1.);
#3229=VECTOR('',#11310,0.225);
#3230=VECTOR('',#11315,0.225);
#3231=VECTOR('',#11320,0.6);
#3232=VECTOR('',#11325,1.);
#3233=VECTOR('',#11326,1.);
#3234=VECTOR('',#11327,1.);
#3235=VECTOR('',#11330,1.);
#3236=VECTOR('',#11331,1.);
#3237=VECTOR('',#11334,1.);
#3238=VECTOR('',#11335,1.);
#3239=VECTOR('',#11338,1.);
#3240=VECTOR('',#11345,0.4);
#3241=VECTOR('',#11348,1.);
#3242=VECTOR('',#11353,1.);
#3243=VECTOR('',#11360,0.165);
#3244=VECTOR('',#11367,1.);
#3245=VECTOR('',#11372,1.);
#3246=VECTOR('',#11375,1.);
#3247=VECTOR('',#11384,1.);
#3248=VECTOR('',#11393,1.);
#3249=VECTOR('',#11394,1.);
#3250=VECTOR('',#11395,1.);
#3251=VECTOR('',#11396,1.);
#3252=VECTOR('',#11397,1.);
#3253=VECTOR('',#11398,1.);
#3254=VECTOR('',#11403,0.225);
#3255=VECTOR('',#11408,0.225);
#3256=VECTOR('',#11413,0.6);
#3257=VECTOR('',#11418,1.);
#3258=VECTOR('',#11419,1.);
#3259=VECTOR('',#11420,1.);
#3260=VECTOR('',#11423,1.);
#3261=VECTOR('',#11424,1.);
#3262=VECTOR('',#11427,1.);
#3263=VECTOR('',#11428,1.);
#3264=VECTOR('',#11431,1.);
#3265=VECTOR('',#11438,1.);
#3266=VECTOR('',#11439,1.);
#3267=VECTOR('',#11440,1.);
#3268=VECTOR('',#11441,1.);
#3269=VECTOR('',#11444,1.);
#3270=VECTOR('',#11445,1.);
#3271=VECTOR('',#11446,1.);
#3272=VECTOR('',#11449,1.);
#3273=VECTOR('',#11450,1.);
#3274=VECTOR('',#11451,1.);
#3275=VECTOR('',#11454,1.);
#3276=VECTOR('',#11455,1.);
#3277=VECTOR('',#11456,1.);
#3278=VECTOR('',#11459,1.);
#3279=VECTOR('',#11460,1.);
#3280=VECTOR('',#11461,1.);
#3281=VECTOR('',#11464,1.);
#3282=VECTOR('',#11465,1.);
#3283=VECTOR('',#11482,0.4);
#3284=VECTOR('',#11487,0.425);
#3285=VECTOR('',#11492,0.41);
#3286=VECTOR('',#11501,0.26);
#3287=VECTOR('',#11504,0.25);
#3288=VECTOR('',#11523,0.976185);
#3289=VECTOR('',#11530,0.5);
#3290=VECTOR('',#11535,0.53);
#3291=VECTOR('',#11544,0.976185);
#3292=VECTOR('',#11551,0.53);
#3293=VECTOR('',#11570,1.023815);
#3294=VECTOR('',#11581,1.47);
#3295=VECTOR('',#11586,1.5);
#3296=VECTOR('',#11591,1.47);
#3297=VECTOR('',#11596,1.023815);
#3298=VECTOR('',#11647,1.019052);
#3299=VECTOR('',#11724,0.980948);
#3300=VECTOR('',#11753,1.013815);
#3301=VECTOR('',#11760,0.991185);
#3302=VECTOR('',#11771,1.013815);
#3303=VECTOR('',#11778,0.991185);
#3304=VECTOR('',#11799,0.55);
#3305=VECTOR('',#11804,0.6);
#3306=VECTOR('',#11811,1.);
#3307=VECTOR('',#11812,1.);
#3308=VECTOR('',#11813,1.);
#3309=VECTOR('',#11814,1.);
#3310=VECTOR('',#11817,1.);
#3311=VECTOR('',#11818,1.);
#3312=VECTOR('',#11819,1.);
#3313=VECTOR('',#11822,1.);
#3314=VECTOR('',#11823,1.);
#3315=VECTOR('',#11824,1.);
#3316=VECTOR('',#11827,1.);
#3317=VECTOR('',#11828,1.);
#3318=VECTOR('',#11829,1.);
#3319=VECTOR('',#11832,1.);
#3320=VECTOR('',#11833,1.);
#3321=VECTOR('',#11834,1.);
#3322=VECTOR('',#11837,1.);
#3323=VECTOR('',#11838,1.);
#3324=VECTOR('',#11849,0.185);
#3325=VECTOR('',#11854,0.2);
#3326=VECTOR('',#11859,0.1625);
#3327=VECTOR('',#11870,0.25);
#3328=VECTOR('',#11877,0.25);
#3329=VECTOR('',#11884,0.225);
#3330=VECTOR('',#11889,1.);
#3331=VECTOR('',#11892,1.);
#3332=VECTOR('',#11897,1.);
#3333=VECTOR('',#11898,1.);
#3334=VECTOR('',#11899,1.);
#3335=VECTOR('',#11902,1.);
#3336=VECTOR('',#11905,1.);
#3337=VECTOR('',#11908,1.);
#3338=VECTOR('',#11911,1.);
#3339=VECTOR('',#11914,1.);
#3340=VECTOR('',#11919,1.);
#3341=VECTOR('',#11920,1.);
#3342=VECTOR('',#11923,1.);
#3343=VECTOR('',#11930,1.);
#3344=VECTOR('',#11933,1.);
#3345=VECTOR('',#11934,1.);
#3346=VECTOR('',#11939,1.);
#3347=VECTOR('',#11940,1.);
#3348=VECTOR('',#11943,1.);
#3349=VECTOR('',#11946,1.);
#3350=VECTOR('',#11949,1.);
#3351=VECTOR('',#11956,1.);
#3352=VECTOR('',#11957,1.);
#3353=VECTOR('',#11960,1.);
#3354=VECTOR('',#11973,0.7);
#3355=VECTOR('',#11976,0.5);
#3356=VECTOR('',#11987,0.165);
#3357=VECTOR('',#11996,0.6);
#3358=VECTOR('',#12009,0.505);
#3359=VECTOR('',#12016,0.7);
#3360=VECTOR('',#12027,1.);
#3361=VECTOR('',#12034,0.165);
#3362=VECTOR('',#12037,1.);
#3363=VECTOR('',#12042,0.505);
#3364=VECTOR('',#12049,0.9);
#3365=VECTOR('',#12062,0.165);
#3366=VECTOR('',#12081,0.7);
#3367=VECTOR('',#12084,0.3);
#3368=VECTOR('',#12091,0.3);
#3369=VECTOR('',#12102,0.305);
#3370=VECTOR('',#12109,0.5);
#3371=VECTOR('',#12122,0.305);
#3372=VECTOR('',#12129,0.5);
#3373=VECTOR('',#12142,0.225);
#3374=VECTOR('',#12149,0.5);
#3375=VECTOR('',#12162,0.165);
#3376=VECTOR('',#12181,0.7);
#3377=VECTOR('',#12184,0.3);
#3378=VECTOR('',#12191,0.3);
#3379=VECTOR('',#12202,0.305);
#3380=VECTOR('',#12209,0.5);
#3381=VECTOR('',#12222,0.305);
#3382=VECTOR('',#12229,0.5);
#3383=VECTOR('',#12242,0.225);
#3384=VECTOR('',#12249,0.5);
#3385=VECTOR('',#12266,0.325);
#3386=VECTOR('',#12271,0.35);
#3387=VECTOR('',#12276,0.335);
#3388=VECTOR('',#12285,0.21);
#3389=VECTOR('',#12290,0.2);
#3390=VECTOR('',#12295,0.18);
#3391=VECTOR('',#12300,1.);
#3392=VECTOR('',#12301,1.);
#3393=VECTOR('',#12302,1.);
#3394=VECTOR('',#12303,1.);
#3395=VECTOR('',#12306,1.);
#3396=VECTOR('',#12307,1.);
#3397=VECTOR('',#12308,1.);
#3398=VECTOR('',#12311,1.);
#3399=VECTOR('',#12312,1.);
#3400=VECTOR('',#12313,1.);
#3401=VECTOR('',#12316,1.);
#3402=VECTOR('',#12317,1.);
#3403=VECTOR('',#12318,1.);
#3404=VECTOR('',#12321,1.);
#3405=VECTOR('',#12322,1.);
#3406=VECTOR('',#12323,1.);
#3407=VECTOR('',#12326,1.);
#3408=VECTOR('',#12327,1.);
#3409=VECTOR('',#12340,1.);
#3410=VECTOR('',#12341,1.);
#3411=VECTOR('',#12342,1.);
#3412=VECTOR('',#12343,1.);
#3413=VECTOR('',#12346,1.);
#3414=VECTOR('',#12347,1.);
#3415=VECTOR('',#12348,1.);
#3416=VECTOR('',#12351,1.);
#3417=VECTOR('',#12352,1.);
#3418=VECTOR('',#12353,1.);
#3419=VECTOR('',#12356,1.);
#3420=VECTOR('',#12357,1.);
#3421=VECTOR('',#12358,1.);
#3422=VECTOR('',#12361,1.);
#3423=VECTOR('',#12362,1.);
#3424=VECTOR('',#12363,1.);
#3425=VECTOR('',#12366,1.);
#3426=VECTOR('',#12367,1.);
#3427=VECTOR('',#12378,0.185);
#3428=VECTOR('',#12381,0.2);
#3429=VECTOR('',#12390,0.5);
#3430=VECTOR('',#12397,0.5);
#3431=VECTOR('',#12402,1.);
#3432=VECTOR('',#12405,1.);
#3433=VECTOR('',#12410,1.);
#3434=VECTOR('',#12411,1.);
#3435=VECTOR('',#12412,1.);
#3436=VECTOR('',#12415,1.);
#3437=VECTOR('',#12420,1.);
#3438=VECTOR('',#12421,1.);
#3439=VECTOR('',#12434,0.305);
#3440=VECTOR('',#12441,0.5);
#3441=VECTOR('',#12454,0.305);
#3442=VECTOR('',#12461,0.5);
#3443=VECTOR('',#12482,0.5);
#3444=VECTOR('',#12489,0.5);
#3445=VECTOR('',#12494,1.);
#3446=VECTOR('',#12497,1.);
#3447=VECTOR('',#12502,1.);
#3448=VECTOR('',#12503,1.);
#3449=VECTOR('',#12504,1.);
#3450=VECTOR('',#12507,1.);
#3451=VECTOR('',#12512,1.);
#3452=VECTOR('',#12513,1.);
#3453=VECTOR('',#12526,0.305);
#3454=VECTOR('',#12533,0.5);
#3455=VECTOR('',#12546,0.305);
#3456=VECTOR('',#12553,0.5);
#3457=VECTOR('',#12574,0.25);
#3458=VECTOR('',#12583,0.165);
#3459=VECTOR('',#12590,0.165);
#3460=VECTOR('',#12597,0.165);
#3461=VECTOR('',#12604,0.165);
#3462=VECTOR('',#12611,1.05);
#3463=VECTOR('',#12616,1.);
#3464=VECTOR('',#12617,1.);
#3465=VECTOR('',#12618,1.);
#3466=VECTOR('',#12619,1.);
#3467=VECTOR('',#12622,1.);
#3468=VECTOR('',#12623,1.);
#3469=VECTOR('',#12624,1.);
#3470=VECTOR('',#12627,1.);
#3471=VECTOR('',#12628,1.);
#3472=VECTOR('',#12629,1.);
#3473=VECTOR('',#12632,1.);
#3474=VECTOR('',#12633,1.);
#3475=VECTOR('',#12644,0.225);
#3476=VECTOR('',#12651,0.225);
#3477=VECTOR('',#12658,0.225);
#3478=VECTOR('',#12665,0.225);
#3479=VECTOR('',#12672,0.7);
#3480=VECTOR('',#12677,1.);
#3481=VECTOR('',#12678,1.);
#3482=VECTOR('',#12679,1.);
#3483=VECTOR('',#12680,1.);
#3484=VECTOR('',#12683,1.);
#3485=VECTOR('',#12684,1.);
#3486=VECTOR('',#12685,1.);
#3487=VECTOR('',#12688,1.);
#3488=VECTOR('',#12689,1.);
#3489=VECTOR('',#12690,1.);
#3490=VECTOR('',#12693,1.);
#3491=VECTOR('',#12694,1.);
#3492=VECTOR('',#12705,0.225);
#3493=VECTOR('',#12712,0.225);
#3494=VECTOR('',#12719,0.225);
#3495=VECTOR('',#12726,0.225);
#3496=VECTOR('',#12733,0.7);
#3497=VECTOR('',#12738,1.);
#3498=VECTOR('',#12739,1.);
#3499=VECTOR('',#12740,1.);
#3500=VECTOR('',#12741,1.);
#3501=VECTOR('',#12744,1.);
#3502=VECTOR('',#12745,1.);
#3503=VECTOR('',#12746,1.);
#3504=VECTOR('',#12749,1.);
#3505=VECTOR('',#12750,1.);
#3506=VECTOR('',#12751,1.);
#3507=VECTOR('',#12754,1.);
#3508=VECTOR('',#12755,1.);
#3509=VECTOR('',#12766,0.164999999999999);
#3510=VECTOR('',#12785,0.699999999999999);
#3511=VECTOR('',#12788,0.300000000000001);
#3512=VECTOR('',#12795,0.300000000000001);
#3513=VECTOR('',#12806,0.305);
#3514=VECTOR('',#12813,0.5);
#3515=VECTOR('',#12826,0.305);
#3516=VECTOR('',#12833,0.5);
#3517=VECTOR('',#12846,0.225);
#3518=VECTOR('',#12853,0.5);
#3519=VECTOR('',#12868,0.25);
#3520=VECTOR('',#12877,0.165);
#3521=VECTOR('',#12884,0.165);
#3522=VECTOR('',#12891,0.165);
#3523=VECTOR('',#12898,0.165);
#3524=VECTOR('',#12905,1.05);
#3525=VECTOR('',#12910,1.);
#3526=VECTOR('',#12911,1.);
#3527=VECTOR('',#12912,1.);
#3528=VECTOR('',#12913,1.);
#3529=VECTOR('',#12916,1.);
#3530=VECTOR('',#12917,1.);
#3531=VECTOR('',#12918,1.);
#3532=VECTOR('',#12921,1.);
#3533=VECTOR('',#12922,1.);
#3534=VECTOR('',#12923,1.);
#3535=VECTOR('',#12926,1.);
#3536=VECTOR('',#12927,1.);
#3537=VECTOR('',#12938,0.225);
#3538=VECTOR('',#12945,0.225);
#3539=VECTOR('',#12952,0.225);
#3540=VECTOR('',#12959,0.225);
#3541=VECTOR('',#12966,0.7);
#3542=VECTOR('',#12971,1.);
#3543=VECTOR('',#12972,1.);
#3544=VECTOR('',#12973,1.);
#3545=VECTOR('',#12974,1.);
#3546=VECTOR('',#12977,1.);
#3547=VECTOR('',#12978,1.);
#3548=VECTOR('',#12979,1.);
#3549=VECTOR('',#12982,1.);
#3550=VECTOR('',#12983,1.);
#3551=VECTOR('',#12984,1.);
#3552=VECTOR('',#12987,1.);
#3553=VECTOR('',#12988,1.);
#3554=VECTOR('',#12999,0.225);
#3555=VECTOR('',#13006,0.225);
#3556=VECTOR('',#13013,0.225);
#3557=VECTOR('',#13020,0.225);
#3558=VECTOR('',#13027,0.7);
#3559=VECTOR('',#13032,1.);
#3560=VECTOR('',#13033,1.);
#3561=VECTOR('',#13034,1.);
#3562=VECTOR('',#13035,1.);
#3563=VECTOR('',#13038,1.);
#3564=VECTOR('',#13039,1.);
#3565=VECTOR('',#13040,1.);
#3566=VECTOR('',#13043,1.);
#3567=VECTOR('',#13044,1.);
#3568=VECTOR('',#13045,1.);
#3569=VECTOR('',#13048,1.);
#3570=VECTOR('',#13049,1.);
#3571=VECTOR('',#13060,0.165);
#3572=VECTOR('',#13079,0.7);
#3573=VECTOR('',#13082,0.3);
#3574=VECTOR('',#13089,0.3);
#3575=VECTOR('',#13100,0.305);
#3576=VECTOR('',#13107,0.5);
#3577=VECTOR('',#13120,0.305);
#3578=VECTOR('',#13127,0.5);
#3579=VECTOR('',#13140,0.225);
#3580=VECTOR('',#13147,0.5);
#3581=VECTOR('',#13162,1.);
#3582=VECTOR('',#13163,1.);
#3583=VECTOR('',#13164,1.);
#3584=VECTOR('',#13167,1.);
#3585=VECTOR('',#13168,1.);
#3586=VECTOR('',#13169,1.);
#3587=VECTOR('',#13174,1.);
#3588=VECTOR('',#13175,1.);
#3589=VECTOR('',#13178,1.);
#3590=VECTOR('',#13179,1.);
#3591=VECTOR('',#13192,1.05);
#3592=VECTOR('',#13201,1.);
#3593=VECTOR('',#13210,1.05);
#3594=VECTOR('',#13219,1.);
#3595=VECTOR('',#13228,1.05);
#3596=VECTOR('',#13235,0.9);
#3597=VECTOR('',#13242,1.);
#3598=VECTOR('',#13245,1.);
#3599=VECTOR('',#13248,1.);
#3600=VECTOR('',#13249,1.);
#3601=VECTOR('',#13250,1.);
#3602=VECTOR('',#13257,1.);
#3603=VECTOR('',#13260,1.);
#3604=VECTOR('',#13261,1.);
#3605=VECTOR('',#13272,0.895);
#3606=VECTOR('',#13279,0.605);
#3607=VECTOR('',#13288,1.);
#3608=VECTOR('',#13289,1.);
#3609=VECTOR('',#13290,1.);
#3610=VECTOR('',#13291,1.);
#3611=VECTOR('',#13294,1.);
#3612=VECTOR('',#13295,1.);
#3613=VECTOR('',#13296,1.);
#3614=VECTOR('',#13299,1.);
#3615=VECTOR('',#13300,1.);
#3616=VECTOR('',#13301,1.);
#3617=VECTOR('',#13304,1.);
#3618=VECTOR('',#13305,1.);
#3619=VECTOR('',#13306,1.);
#3620=VECTOR('',#13309,1.);
#3621=VECTOR('',#13310,1.);
#3622=VECTOR('',#13311,1.);
#3623=VECTOR('',#13314,1.);
#3624=VECTOR('',#13315,1.);
#3625=VECTOR('',#13332,0.325);
#3626=VECTOR('',#13337,0.35);
#3627=VECTOR('',#13342,0.335);
#3628=VECTOR('',#13351,0.21);
#3629=VECTOR('',#13354,0.2);
#3630=CIRCLE('',#9458,0.165);
#3631=CIRCLE('',#9459,0.165);
#3632=CIRCLE('',#9461,0.165);
#3633=CIRCLE('',#9462,0.165);
#3634=CIRCLE('',#9464,0.165);
#3635=CIRCLE('',#9465,0.165);
#3636=CIRCLE('',#9467,0.165);
#3637=CIRCLE('',#9468,0.165);
#3638=CIRCLE('',#9470,0.164999999999999);
#3639=CIRCLE('',#9471,0.164999999999999);
#3640=CIRCLE('',#9473,0.164999999999999);
#3641=CIRCLE('',#9474,0.164999999999999);
#3642=CIRCLE('',#9476,0.165);
#3643=CIRCLE('',#9477,0.165);
#3644=CIRCLE('',#9479,0.165);
#3645=CIRCLE('',#9480,0.165);
#3646=CIRCLE('',#9482,0.21);
#3647=CIRCLE('',#9483,0.21);
#3648=CIRCLE('',#9485,0.21);
#3649=CIRCLE('',#9486,0.21);
#3650=CIRCLE('',#9488,0.21);
#3651=CIRCLE('',#9489,0.21);
#3652=CIRCLE('',#9491,0.21);
#3653=CIRCLE('',#9492,0.21);
#3654=CIRCLE('',#9516,0.165);
#3655=CIRCLE('',#9517,0.165);
#3656=CIRCLE('',#9520,0.165);
#3657=CIRCLE('',#9521,0.165);
#3658=CIRCLE('',#9524,0.165);
#3659=CIRCLE('',#9525,0.165);
#3660=CIRCLE('',#9528,0.165);
#3661=CIRCLE('',#9529,0.165);
#3662=CIRCLE('',#9532,2.2);
#3663=CIRCLE('',#9533,0.525);
#3664=CIRCLE('',#9535,0.525);
#3665=CIRCLE('',#9537,0.525);
#3666=CIRCLE('',#9538,0.525);
#3667=CIRCLE('',#9540,2.2);
#3668=CIRCLE('',#9542,0.525);
#3669=CIRCLE('',#9543,0.525);
#3670=CIRCLE('',#9545,2.2);
#3671=CIRCLE('',#9547,0.525);
#3672=CIRCLE('',#9548,0.525);
#3673=CIRCLE('',#9550,2.2);
#3674=CIRCLE('',#9552,2.2);
#3675=CIRCLE('',#9553,2.2);
#3676=CIRCLE('',#9554,2.2);
#3677=CIRCLE('',#9555,2.2);
#3678=CIRCLE('',#9556,2.2);
#3679=CIRCLE('',#9557,2.2);
#3680=CIRCLE('',#9559,3.);
#3681=CIRCLE('',#9560,0.275);
#3682=CIRCLE('',#9561,0.275);
#3683=CIRCLE('',#9562,0.275);
#3684=CIRCLE('',#9563,0.275);
#3685=CIRCLE('',#9565,0.275);
#3686=CIRCLE('',#9567,0.275);
#3687=CIRCLE('',#9569,0.275);
#3688=CIRCLE('',#9571,0.275);
#3689=CIRCLE('',#9573,1.5);
#3690=CIRCLE('',#9574,1.5);
#3691=CIRCLE('',#9576,1.02);
#3692=CIRCLE('',#9578,3.);
#3693=CIRCLE('',#9580,1.02);
#3694=CIRCLE('',#9585,0.375);
#3695=CIRCLE('',#9586,0.375);
#3696=CIRCLE('',#9588,0.225);
#3697=CIRCLE('',#9590,0.375);
#3698=CIRCLE('',#9591,0.375);
#3699=CIRCLE('',#9593,0.225);
#3700=CIRCLE('',#9595,0.375);
#3701=CIRCLE('',#9596,0.375);
#3702=CIRCLE('',#9598,0.225);
#3703=CIRCLE('',#9600,0.375);
#3704=CIRCLE('',#9601,0.375);
#3705=CIRCLE('',#9603,0.225);
#3706=CIRCLE('',#9605,0.225);
#3707=CIRCLE('',#9607,0.225);
#3708=CIRCLE('',#9609,0.225);
#3709=CIRCLE('',#9611,0.225);
#3710=CIRCLE('',#9613,1.49);
#3711=CIRCLE('',#9614,1.49);
#3712=CIRCLE('',#9616,0.71);
#3713=CIRCLE('',#9618,0.71);
#3714=CIRCLE('',#9620,2.2);
#3715=CIRCLE('',#9621,2.2);
#3716=CIRCLE('',#9626,0.4);
#3717=CIRCLE('',#9627,0.4);
#3718=CIRCLE('',#9629,0.4);
#3719=CIRCLE('',#9630,0.4);
#3720=CIRCLE('',#9632,0.165);
#3721=CIRCLE('',#9634,0.165);
#3722=CIRCLE('',#9635,0.165);
#3723=CIRCLE('',#9638,0.4);
#3724=CIRCLE('',#9639,0.4);
#3725=CIRCLE('',#9641,0.225);
#3726=CIRCLE('',#9643,0.4);
#3727=CIRCLE('',#9644,0.4);
#3728=CIRCLE('',#9646,0.225);
#3729=CIRCLE('',#9649,0.225);
#3730=CIRCLE('',#9651,0.225);
#3731=CIRCLE('',#9653,0.6);
#3732=CIRCLE('',#9654,0.6);
#3733=CIRCLE('',#9662,0.4);
#3734=CIRCLE('',#9663,0.4);
#3735=CIRCLE('',#9665,0.4);
#3736=CIRCLE('',#9666,0.4);
#3737=CIRCLE('',#9668,0.164999999999999);
#3738=CIRCLE('',#9670,0.164999999999999);
#3739=CIRCLE('',#9671,0.164999999999999);
#3740=CIRCLE('',#9674,0.4);
#3741=CIRCLE('',#9675,0.4);
#3742=CIRCLE('',#9677,0.225);
#3743=CIRCLE('',#9679,0.4);
#3744=CIRCLE('',#9680,0.4);
#3745=CIRCLE('',#9682,0.225);
#3746=CIRCLE('',#9685,0.225);
#3747=CIRCLE('',#9687,0.225);
#3748=CIRCLE('',#9689,0.6);
#3749=CIRCLE('',#9690,0.6);
#3750=CIRCLE('',#9698,0.4);
#3751=CIRCLE('',#9699,0.4);
#3752=CIRCLE('',#9701,0.165);
#3753=CIRCLE('',#9703,0.165);
#3754=CIRCLE('',#9704,0.165);
#3755=CIRCLE('',#9705,0.165);
#3756=CIRCLE('',#9708,0.4);
#3757=CIRCLE('',#9709,0.4);
#3758=CIRCLE('',#9711,0.225);
#3759=CIRCLE('',#9713,0.4);
#3760=CIRCLE('',#9714,0.4);
#3761=CIRCLE('',#9716,0.225);
#3762=CIRCLE('',#9719,0.225);
#3763=CIRCLE('',#9721,0.225);
#3764=CIRCLE('',#9723,0.6);
#3765=CIRCLE('',#9724,0.6);
#3766=CIRCLE('',#9732,0.4);
#3767=CIRCLE('',#9733,0.4);
#3768=CIRCLE('',#9735,0.165);
#3769=CIRCLE('',#9737,0.165);
#3770=CIRCLE('',#9738,0.165);
#3771=CIRCLE('',#9739,0.165);
#3772=CIRCLE('',#9742,0.4);
#3773=CIRCLE('',#9743,0.4);
#3774=CIRCLE('',#9745,0.225);
#3775=CIRCLE('',#9747,0.4);
#3776=CIRCLE('',#9748,0.4);
#3777=CIRCLE('',#9750,0.225);
#3778=CIRCLE('',#9753,0.225);
#3779=CIRCLE('',#9755,0.225);
#3780=CIRCLE('',#9757,0.6);
#3781=CIRCLE('',#9758,0.6);
#3782=CIRCLE('',#9774,0.24505);
#3783=CIRCLE('',#9776,0.375);
#3784=CIRCLE('',#9778,0.425);
#3785=CIRCLE('',#9780,0.425);
#3786=CIRCLE('',#9782,0.395);
#3787=CIRCLE('',#9784,0.27);
#3788=CIRCLE('',#9786,0.24505);
#3789=CIRCLE('',#9791,0.976185);
#3790=CIRCLE('',#9792,0.976185);
#3791=CIRCLE('',#9793,0.247676);
#3792=CIRCLE('',#9794,0.976185);
#3793=CIRCLE('',#9795,0.976185);
#3794=CIRCLE('',#9797,0.976185);
#3795=CIRCLE('',#9799,0.5);
#3796=CIRCLE('',#9800,0.5);
#3797=CIRCLE('',#9802,0.56);
#3798=CIRCLE('',#9805,0.976185);
#3799=CIRCLE('',#9807,0.56);
#3800=CIRCLE('',#9811,1.023815);
#3801=CIRCLE('',#9812,1.023815);
#3802=CIRCLE('',#9813,0.247676);
#3803=CIRCLE('',#9814,1.023815);
#3804=CIRCLE('',#9815,1.023815);
#3805=CIRCLE('',#9817,1.023815);
#3806=CIRCLE('',#9819,1.44);
#3807=CIRCLE('',#9820,1.023815);
#3808=CIRCLE('',#9822,1.5);
#3809=CIRCLE('',#9824,1.5);
#3810=CIRCLE('',#9826,1.44);
#3811=CIRCLE('',#9831,0.23815);
#3812=CIRCLE('',#9833,0.23815);
#3813=CIRCLE('',#9835,0.23815);
#3814=CIRCLE('',#9837,0.23815);
#3815=CIRCLE('',#9839,0.23815);
#3816=CIRCLE('',#9841,0.23815);
#3817=CIRCLE('',#9843,0.23815);
#3818=CIRCLE('',#9845,0.23815);
#3819=CIRCLE('',#9848,0.243053047864041);
#3820=CIRCLE('',#9849,0.243053047864041);
#3821=CIRCLE('',#9851,1.019052);
#3822=CIRCLE('',#9852,1.019052);
#3823=CIRCLE('',#9853,1.019052);
#3824=CIRCLE('',#9854,1.019052);
#3825=CIRCLE('',#9855,1.019052);
#3826=CIRCLE('',#9856,1.019052);
#3827=CIRCLE('',#9857,1.019052);
#3828=CIRCLE('',#9858,1.019052);
#3829=CIRCLE('',#9859,1.019052);
#3830=CIRCLE('',#9861,0.980948);
#3831=CIRCLE('',#9862,0.243053047864041);
#3832=CIRCLE('',#9864,0.243053047864041);
#3833=CIRCLE('',#9866,0.980948);
#3834=CIRCLE('',#9867,0.243053047864041);
#3835=CIRCLE('',#9869,0.243053047864041);
#3836=CIRCLE('',#9871,0.980948);
#3837=CIRCLE('',#9872,0.243053047864041);
#3838=CIRCLE('',#9874,0.243053047864041);
#3839=CIRCLE('',#9876,0.980948);
#3840=CIRCLE('',#9877,0.243053047864041);
#3841=CIRCLE('',#9879,0.243053047864041);
#3842=CIRCLE('',#9881,0.980948);
#3843=CIRCLE('',#9882,0.243053047864041);
#3844=CIRCLE('',#9884,0.243053047864041);
#3845=CIRCLE('',#9886,0.980948);
#3846=CIRCLE('',#9887,0.243053047864041);
#3847=CIRCLE('',#9889,0.243053047864041);
#3848=CIRCLE('',#9891,0.980948);
#3849=CIRCLE('',#9892,0.980948);
#3850=CIRCLE('',#9893,0.980948);
#3851=CIRCLE('',#9895,0.243053047864041);
#3852=CIRCLE('',#9897,0.243053047864041);
#3853=CIRCLE('',#9902,1.013815);
#3854=CIRCLE('',#9903,0.991185);
#3855=CIRCLE('',#9905,1.013815);
#3856=CIRCLE('',#9907,0.991185);
#3857=CIRCLE('',#9910,1.013815);
#3858=CIRCLE('',#9911,0.991185);
#3859=CIRCLE('',#9913,1.013815);
#3860=CIRCLE('',#9915,0.991185);
#3861=CIRCLE('',#9924,0.6);
#3862=CIRCLE('',#9926,0.6);
#3863=CIRCLE('',#9927,0.5);
#3864=CIRCLE('',#9939,0.17);
#3865=CIRCLE('',#9941,0.1954);
#3866=CIRCLE('',#9943,0.1954);
#3867=CIRCLE('',#9945,0.125);
#3868=CIRCLE('',#9950,0.25);
#3869=CIRCLE('',#9951,0.25);
#3870=CIRCLE('',#9953,0.25);
#3871=CIRCLE('',#9954,0.25);
#3872=CIRCLE('',#9956,0.225);
#3873=CIRCLE('',#9957,0.225);
#3874=CIRCLE('',#9959,0.8);
#3875=CIRCLE('',#9960,0.8);
#3876=CIRCLE('',#9963,1.);
#3877=CIRCLE('',#9964,0.8);
#3878=CIRCLE('',#9965,1.);
#3879=CIRCLE('',#9966,0.8);
#3880=CIRCLE('',#9967,1.);
#3881=CIRCLE('',#9970,1.);
#3882=CIRCLE('',#9972,1.);
#3883=CIRCLE('',#9974,0.8);
#3884=CIRCLE('',#9977,0.8);
#3885=CIRCLE('',#9978,1.);
#3886=CIRCLE('',#9979,0.7);
#3887=CIRCLE('',#9986,0.7);
#3888=CIRCLE('',#9987,0.5);
#3889=CIRCLE('',#9990,0.5);
#3890=CIRCLE('',#9994,0.165);
#3891=CIRCLE('',#9995,0.165);
#3892=CIRCLE('',#9998,0.6);
#3893=CIRCLE('',#9999,0.6);
#3894=CIRCLE('',#10004,0.505);
#3895=CIRCLE('',#10005,0.505);
#3896=CIRCLE('',#10007,0.7);
#3897=CIRCLE('',#10008,0.7);
#3898=CIRCLE('',#10013,0.165);
#3899=CIRCLE('',#10015,0.165);
#3900=CIRCLE('',#10018,0.505);
#3901=CIRCLE('',#10019,0.505);
#3902=CIRCLE('',#10021,0.9);
#3903=CIRCLE('',#10022,0.9);
#3904=CIRCLE('',#10027,0.165);
#3905=CIRCLE('',#10028,0.165);
#3906=CIRCLE('',#10031,0.7);
#3907=CIRCLE('',#10032,0.3);
#3908=CIRCLE('',#10034,0.7);
#3909=CIRCLE('',#10035,0.3);
#3910=CIRCLE('',#10038,0.3);
#3911=CIRCLE('',#10040,0.3);
#3912=CIRCLE('',#10045,0.305);
#3913=CIRCLE('',#10046,0.305);
#3914=CIRCLE('',#10048,0.5);
#3915=CIRCLE('',#10049,0.5);
#3916=CIRCLE('',#10054,0.305);
#3917=CIRCLE('',#10055,0.305);
#3918=CIRCLE('',#10057,0.5);
#3919=CIRCLE('',#10058,0.5);
#3920=CIRCLE('',#10063,0.225);
#3921=CIRCLE('',#10064,0.225);
#3922=CIRCLE('',#10066,0.5);
#3923=CIRCLE('',#10067,0.5);
#3924=CIRCLE('',#10072,0.165);
#3925=CIRCLE('',#10073,0.165);
#3926=CIRCLE('',#10076,0.7);
#3927=CIRCLE('',#10077,0.3);
#3928=CIRCLE('',#10079,0.7);
#3929=CIRCLE('',#10080,0.3);
#3930=CIRCLE('',#10083,0.3);
#3931=CIRCLE('',#10085,0.3);
#3932=CIRCLE('',#10090,0.305);
#3933=CIRCLE('',#10091,0.305);
#3934=CIRCLE('',#10093,0.5);
#3935=CIRCLE('',#10094,0.5);
#3936=CIRCLE('',#10099,0.305);
#3937=CIRCLE('',#10100,0.305);
#3938=CIRCLE('',#10102,0.5);
#3939=CIRCLE('',#10103,0.5);
#3940=CIRCLE('',#10108,0.225);
#3941=CIRCLE('',#10109,0.225);
#3942=CIRCLE('',#10111,0.5);
#3943=CIRCLE('',#10112,0.5);
#3944=CIRCLE('',#10117,0.3);
#3945=CIRCLE('',#10119,0.35);
#3946=CIRCLE('',#10121,0.35);
#3947=CIRCLE('',#10123,0.32);
#3948=CIRCLE('',#10125,0.22);
#3949=CIRCLE('',#10127,0.1954);
#3950=CIRCLE('',#10129,0.1954);
#3951=CIRCLE('',#10131,0.16);
#3952=CIRCLE('',#10143,0.1954);
#3953=CIRCLE('',#10152,0.17);
#3954=CIRCLE('',#10154,0.1954);
#3955=CIRCLE('',#10159,0.5);
#3956=CIRCLE('',#10160,0.5);
#3957=CIRCLE('',#10162,0.5);
#3958=CIRCLE('',#10163,0.5);
#3959=CIRCLE('',#10165,0.800000000000001);
#3960=CIRCLE('',#10166,0.800000000000001);
#3961=CIRCLE('',#10169,0.8);
#3962=CIRCLE('',#10172,0.8);
#3963=CIRCLE('',#10176,0.305);
#3964=CIRCLE('',#10177,0.305);
#3965=CIRCLE('',#10179,0.5);
#3966=CIRCLE('',#10180,0.5);
#3967=CIRCLE('',#10185,0.305);
#3968=CIRCLE('',#10186,0.305);
#3969=CIRCLE('',#10188,0.5);
#3970=CIRCLE('',#10189,0.5);
#3971=CIRCLE('',#10198,0.5);
#3972=CIRCLE('',#10199,0.5);
#3973=CIRCLE('',#10201,0.5);
#3974=CIRCLE('',#10202,0.5);
#3975=CIRCLE('',#10204,0.8);
#3976=CIRCLE('',#10205,0.8);
#3977=CIRCLE('',#10208,0.8);
#3978=CIRCLE('',#10211,0.8);
#3979=CIRCLE('',#10215,0.305);
#3980=CIRCLE('',#10216,0.305);
#3981=CIRCLE('',#10218,0.5);
#3982=CIRCLE('',#10219,0.5);
#3983=CIRCLE('',#10224,0.305);
#3984=CIRCLE('',#10225,0.305);
#3985=CIRCLE('',#10227,0.5);
#3986=CIRCLE('',#10228,0.5);
#3987=CIRCLE('',#10237,0.25);
#3988=CIRCLE('',#10238,0.25);
#3989=CIRCLE('',#10241,0.165);
#3990=CIRCLE('',#10242,0.165);
#3991=CIRCLE('',#10244,0.165);
#3992=CIRCLE('',#10245,0.165);
#3993=CIRCLE('',#10247,0.165);
#3994=CIRCLE('',#10248,0.165);
#3995=CIRCLE('',#10250,0.165);
#3996=CIRCLE('',#10251,0.165);
#3997=CIRCLE('',#10253,1.05);
#3998=CIRCLE('',#10254,1.05);
#3999=CIRCLE('',#10263,0.225);
#4000=CIRCLE('',#10264,0.225);
#4001=CIRCLE('',#10266,0.225);
#4002=CIRCLE('',#10267,0.225);
#4003=CIRCLE('',#10269,0.225);
#4004=CIRCLE('',#10270,0.225);
#4005=CIRCLE('',#10272,0.225);
#4006=CIRCLE('',#10273,0.225);
#4007=CIRCLE('',#10275,0.7);
#4008=CIRCLE('',#10276,0.7);
#4009=CIRCLE('',#10285,0.225);
#4010=CIRCLE('',#10286,0.225);
#4011=CIRCLE('',#10288,0.225);
#4012=CIRCLE('',#10289,0.225);
#4013=CIRCLE('',#10291,0.225);
#4014=CIRCLE('',#10292,0.225);
#4015=CIRCLE('',#10294,0.225);
#4016=CIRCLE('',#10295,0.225);
#4017=CIRCLE('',#10297,0.7);
#4018=CIRCLE('',#10298,0.7);
#4019=CIRCLE('',#10307,0.164999999999999);
#4020=CIRCLE('',#10308,0.164999999999999);
#4021=CIRCLE('',#10311,0.699999999999999);
#4022=CIRCLE('',#10312,0.300000000000001);
#4023=CIRCLE('',#10314,0.699999999999999);
#4024=CIRCLE('',#10315,0.300000000000001);
#4025=CIRCLE('',#10318,0.300000000000001);
#4026=CIRCLE('',#10320,0.300000000000001);
#4027=CIRCLE('',#10325,0.305);
#4028=CIRCLE('',#10326,0.305);
#4029=CIRCLE('',#10328,0.5);
#4030=CIRCLE('',#10329,0.5);
#4031=CIRCLE('',#10334,0.305);
#4032=CIRCLE('',#10335,0.305);
#4033=CIRCLE('',#10337,0.5);
#4034=CIRCLE('',#10338,0.5);
#4035=CIRCLE('',#10343,0.225);
#4036=CIRCLE('',#10344,0.225);
#4037=CIRCLE('',#10346,0.5);
#4038=CIRCLE('',#10347,0.5);
#4039=CIRCLE('',#10353,0.25);
#4040=CIRCLE('',#10354,0.25);
#4041=CIRCLE('',#10357,0.165);
#4042=CIRCLE('',#10358,0.165);
#4043=CIRCLE('',#10360,0.165);
#4044=CIRCLE('',#10361,0.165);
#4045=CIRCLE('',#10363,0.165);
#4046=CIRCLE('',#10364,0.165);
#4047=CIRCLE('',#10366,0.165);
#4048=CIRCLE('',#10367,0.165);
#4049=CIRCLE('',#10369,1.05);
#4050=CIRCLE('',#10370,1.05);
#4051=CIRCLE('',#10379,0.225);
#4052=CIRCLE('',#10380,0.225);
#4053=CIRCLE('',#10382,0.225);
#4054=CIRCLE('',#10383,0.225);
#4055=CIRCLE('',#10385,0.225);
#4056=CIRCLE('',#10386,0.225);
#4057=CIRCLE('',#10388,0.225);
#4058=CIRCLE('',#10389,0.225);
#4059=CIRCLE('',#10391,0.7);
#4060=CIRCLE('',#10392,0.7);
#4061=CIRCLE('',#10401,0.225);
#4062=CIRCLE('',#10402,0.225);
#4063=CIRCLE('',#10404,0.225);
#4064=CIRCLE('',#10405,0.225);
#4065=CIRCLE('',#10407,0.225);
#4066=CIRCLE('',#10408,0.225);
#4067=CIRCLE('',#10410,0.225);
#4068=CIRCLE('',#10411,0.225);
#4069=CIRCLE('',#10413,0.7);
#4070=CIRCLE('',#10414,0.7);
#4071=CIRCLE('',#10423,0.165);
#4072=CIRCLE('',#10424,0.165);
#4073=CIRCLE('',#10427,0.7);
#4074=CIRCLE('',#10428,0.3);
#4075=CIRCLE('',#10430,0.7);
#4076=CIRCLE('',#10431,0.3);
#4077=CIRCLE('',#10434,0.3);
#4078=CIRCLE('',#10436,0.3);
#4079=CIRCLE('',#10441,0.305);
#4080=CIRCLE('',#10442,0.305);
#4081=CIRCLE('',#10444,0.5);
#4082=CIRCLE('',#10445,0.5);
#4083=CIRCLE('',#10450,0.305);
#4084=CIRCLE('',#10451,0.305);
#4085=CIRCLE('',#10453,0.5);
#4086=CIRCLE('',#10454,0.5);
#4087=CIRCLE('',#10459,0.225);
#4088=CIRCLE('',#10460,0.225);
#4089=CIRCLE('',#10462,0.5);
#4090=CIRCLE('',#10463,0.5);
#4091=CIRCLE('',#10469,0.9);
#4092=CIRCLE('',#10472,0.9);
#4093=CIRCLE('',#10476,1.05);
#4094=CIRCLE('',#10477,0.9);
#4095=CIRCLE('',#10479,1.05);
#4096=CIRCLE('',#10481,1.);
#4097=CIRCLE('',#10483,1.);
#4098=CIRCLE('',#10485,1.05);
#4099=CIRCLE('',#10487,1.05);
#4100=CIRCLE('',#10489,1.);
#4101=CIRCLE('',#10491,1.);
#4102=CIRCLE('',#10493,1.05);
#4103=CIRCLE('',#10495,1.05);
#4104=CIRCLE('',#10497,0.9);
#4105=CIRCLE('',#10501,0.895);
#4106=CIRCLE('',#10502,0.605);
#4107=CIRCLE('',#10505,0.895);
#4108=CIRCLE('',#10506,0.605);
#4109=CIRCLE('',#10509,0.895);
#4110=CIRCLE('',#10510,0.605);
#4111=CIRCLE('',#10512,0.895);
#4112=CIRCLE('',#10514,0.605);
#4113=CIRCLE('',#10528,0.1954);
#4114=CIRCLE('',#10530,0.3);
#4115=CIRCLE('',#10532,0.35);
#4116=CIRCLE('',#10534,0.35);
#4117=CIRCLE('',#10536,0.32);
#4118=CIRCLE('',#10538,0.22);
#4119=CIRCLE('',#10540,0.1954);
#4120=VERTEX_POINT('',#13535);
#4121=VERTEX_POINT('',#13537);
#4122=VERTEX_POINT('',#13541);
#4123=VERTEX_POINT('',#13543);
#4124=VERTEX_POINT('',#13547);
#4125=VERTEX_POINT('',#13549);
#4126=VERTEX_POINT('',#13553);
#4127=VERTEX_POINT('',#13555);
#4128=VERTEX_POINT('',#13559);
#4129=VERTEX_POINT('',#13561);
#4130=VERTEX_POINT('',#13565);
#4131=VERTEX_POINT('',#13567);
#4132=VERTEX_POINT('',#13571);
#4133=VERTEX_POINT('',#13573);
#4134=VERTEX_POINT('',#13577);
#4135=VERTEX_POINT('',#13579);
#4136=VERTEX_POINT('',#13583);
#4137=VERTEX_POINT('',#13585);
#4138=VERTEX_POINT('',#13589);
#4139=VERTEX_POINT('',#13591);
#4140=VERTEX_POINT('',#13595);
#4141=VERTEX_POINT('',#13597);
#4142=VERTEX_POINT('',#13601);
#4143=VERTEX_POINT('',#13603);
#4144=VERTEX_POINT('',#13607);
#4145=VERTEX_POINT('',#13608);
#4146=VERTEX_POINT('',#13610);
#4147=VERTEX_POINT('',#13612);
#4148=VERTEX_POINT('',#13616);
#4149=VERTEX_POINT('',#13618);
#4150=VERTEX_POINT('',#13622);
#4151=VERTEX_POINT('',#13624);
#4152=VERTEX_POINT('',#13634);
#4153=VERTEX_POINT('',#13635);
#4154=VERTEX_POINT('',#13637);
#4155=VERTEX_POINT('',#13639);
#4156=VERTEX_POINT('',#13643);
#4157=VERTEX_POINT('',#13645);
#4158=VERTEX_POINT('',#13649);
#4159=VERTEX_POINT('',#13651);
#4160=VERTEX_POINT('',#13661);
#4161=VERTEX_POINT('',#13662);
#4162=VERTEX_POINT('',#13664);
#4163=VERTEX_POINT('',#13666);
#4164=VERTEX_POINT('',#13670);
#4165=VERTEX_POINT('',#13672);
#4166=VERTEX_POINT('',#13676);
#4167=VERTEX_POINT('',#13678);
#4168=VERTEX_POINT('',#13688);
#4169=VERTEX_POINT('',#13689);
#4170=VERTEX_POINT('',#13726);
#4171=VERTEX_POINT('',#13728);
#4172=VERTEX_POINT('',#13766);
#4173=VERTEX_POINT('',#13768);
#4174=VERTEX_POINT('',#13773);
#4175=VERTEX_POINT('',#13775);
#4176=VERTEX_POINT('',#13780);
#4177=VERTEX_POINT('',#13782);
#4178=VERTEX_POINT('',#13787);
#4179=VERTEX_POINT('',#13789);
#4180=VERTEX_POINT('',#13794);
#4181=VERTEX_POINT('',#13795);
#4182=VERTEX_POINT('',#13799);
#4183=VERTEX_POINT('',#13801);
#4184=VERTEX_POINT('',#13805);
#4185=VERTEX_POINT('',#13806);
#4186=VERTEX_POINT('',#13808);
#4187=VERTEX_POINT('',#13810);
#4188=VERTEX_POINT('',#13816);
#4189=VERTEX_POINT('',#13817);
#4190=VERTEX_POINT('',#13819);
#4191=VERTEX_POINT('',#13821);
#4192=VERTEX_POINT('',#13827);
#4193=VERTEX_POINT('',#13828);
#4194=VERTEX_POINT('',#13830);
#4195=VERTEX_POINT('',#13832);
#4196=VERTEX_POINT('',#13838);
#4197=VERTEX_POINT('',#13840);
#4198=VERTEX_POINT('',#13848);
#4199=VERTEX_POINT('',#13850);
#4200=VERTEX_POINT('',#13852);
#4201=VERTEX_POINT('',#13854);
#4202=VERTEX_POINT('',#13856);
#4203=VERTEX_POINT('',#13859);
#4204=VERTEX_POINT('',#13863);
#4205=VERTEX_POINT('',#13867);
#4206=VERTEX_POINT('',#13871);
#4207=VERTEX_POINT('',#13875);
#4208=VERTEX_POINT('',#13877);
#4209=VERTEX_POINT('',#13881);
#4210=VERTEX_POINT('',#13884);
#4211=VERTEX_POINT('',#13888);
#4212=VERTEX_POINT('',#13895);
#4213=VERTEX_POINT('',#13897);
#4214=VERTEX_POINT('',#13901);
#4215=VERTEX_POINT('',#13904);
#4216=VERTEX_POINT('',#13906);
#4217=VERTEX_POINT('',#13910);
#4218=VERTEX_POINT('',#13913);
#4219=VERTEX_POINT('',#13915);
#4220=VERTEX_POINT('',#13919);
#4221=VERTEX_POINT('',#13922);
#4222=VERTEX_POINT('',#13924);
#4223=VERTEX_POINT('',#13928);
#4224=VERTEX_POINT('',#13931);
#4225=VERTEX_POINT('',#13935);
#4226=VERTEX_POINT('',#13939);
#4227=VERTEX_POINT('',#13943);
#4228=VERTEX_POINT('',#13947);
#4229=VERTEX_POINT('',#13949);
#4230=VERTEX_POINT('',#13953);
#4231=VERTEX_POINT('',#13956);
#4232=VERTEX_POINT('',#13960);
#4233=VERTEX_POINT('',#13962);
#4234=VERTEX_POINT('',#13969);
#4235=VERTEX_POINT('',#13970);
#4236=VERTEX_POINT('',#13972);
#4237=VERTEX_POINT('',#13974);
#4238=VERTEX_POINT('',#13978);
#4239=VERTEX_POINT('',#13979);
#4240=VERTEX_POINT('',#13981);
#4241=VERTEX_POINT('',#13983);
#4242=VERTEX_POINT('',#13987);
#4243=VERTEX_POINT('',#13988);
#4244=VERTEX_POINT('',#13992);
#4245=VERTEX_POINT('',#13993);
#4246=VERTEX_POINT('',#14000);
#4247=VERTEX_POINT('',#14002);
#4248=VERTEX_POINT('',#14021);
#4249=VERTEX_POINT('',#14031);
#4250=VERTEX_POINT('',#14038);
#4251=VERTEX_POINT('',#14041);
#4252=VERTEX_POINT('',#14042);
#4253=VERTEX_POINT('',#14045);
#4254=VERTEX_POINT('',#14047);
#4255=VERTEX_POINT('',#14052);
#4256=VERTEX_POINT('',#14056);
#4257=VERTEX_POINT('',#14060);
#4258=VERTEX_POINT('',#14063);
#4259=VERTEX_POINT('',#14067);
#4260=VERTEX_POINT('',#14068);
#4261=VERTEX_POINT('',#14073);
#4262=VERTEX_POINT('',#14077);
#4263=VERTEX_POINT('',#14085);
#4264=VERTEX_POINT('',#14086);
#4265=VERTEX_POINT('',#14088);
#4266=VERTEX_POINT('',#14090);
#4267=VERTEX_POINT('',#14094);
#4268=VERTEX_POINT('',#14095);
#4269=VERTEX_POINT('',#14097);
#4270=VERTEX_POINT('',#14099);
#4271=VERTEX_POINT('',#14103);
#4272=VERTEX_POINT('',#14104);
#4273=VERTEX_POINT('',#14108);
#4274=VERTEX_POINT('',#14109);
#4275=VERTEX_POINT('',#14116);
#4276=VERTEX_POINT('',#14118);
#4277=VERTEX_POINT('',#14137);
#4278=VERTEX_POINT('',#14147);
#4279=VERTEX_POINT('',#14154);
#4280=VERTEX_POINT('',#14157);
#4281=VERTEX_POINT('',#14158);
#4282=VERTEX_POINT('',#14161);
#4283=VERTEX_POINT('',#14163);
#4284=VERTEX_POINT('',#14168);
#4285=VERTEX_POINT('',#14172);
#4286=VERTEX_POINT('',#14176);
#4287=VERTEX_POINT('',#14179);
#4288=VERTEX_POINT('',#14183);
#4289=VERTEX_POINT('',#14184);
#4290=VERTEX_POINT('',#14189);
#4291=VERTEX_POINT('',#14193);
#4292=VERTEX_POINT('',#14201);
#4293=VERTEX_POINT('',#14202);
#4294=VERTEX_POINT('',#14204);
#4295=VERTEX_POINT('',#14206);
#4296=VERTEX_POINT('',#14210);
#4297=VERTEX_POINT('',#14211);
#4298=VERTEX_POINT('',#14215);
#4299=VERTEX_POINT('',#14226);
#4300=VERTEX_POINT('',#14228);
#4301=VERTEX_POINT('',#14231);
#4302=VERTEX_POINT('',#14246);
#4303=VERTEX_POINT('',#14248);
#4304=VERTEX_POINT('',#14253);
#4305=VERTEX_POINT('',#14260);
#4306=VERTEX_POINT('',#14263);
#4307=VERTEX_POINT('',#14265);
#4308=VERTEX_POINT('',#14267);
#4309=VERTEX_POINT('',#14270);
#4310=VERTEX_POINT('',#14274);
#4311=VERTEX_POINT('',#14278);
#4312=VERTEX_POINT('',#14282);
#4313=VERTEX_POINT('',#14284);
#4314=VERTEX_POINT('',#14288);
#4315=VERTEX_POINT('',#14289);
#4316=VERTEX_POINT('',#14294);
#4317=VERTEX_POINT('',#14298);
#4318=VERTEX_POINT('',#14306);
#4319=VERTEX_POINT('',#14307);
#4320=VERTEX_POINT('',#14309);
#4321=VERTEX_POINT('',#14311);
#4322=VERTEX_POINT('',#14315);
#4323=VERTEX_POINT('',#14316);
#4324=VERTEX_POINT('',#14320);
#4325=VERTEX_POINT('',#14331);
#4326=VERTEX_POINT('',#14333);
#4327=VERTEX_POINT('',#14336);
#4328=VERTEX_POINT('',#14351);
#4329=VERTEX_POINT('',#14353);
#4330=VERTEX_POINT('',#14358);
#4331=VERTEX_POINT('',#14365);
#4332=VERTEX_POINT('',#14368);
#4333=VERTEX_POINT('',#14370);
#4334=VERTEX_POINT('',#14372);
#4335=VERTEX_POINT('',#14375);
#4336=VERTEX_POINT('',#14379);
#4337=VERTEX_POINT('',#14383);
#4338=VERTEX_POINT('',#14387);
#4339=VERTEX_POINT('',#14389);
#4340=VERTEX_POINT('',#14393);
#4341=VERTEX_POINT('',#14394);
#4342=VERTEX_POINT('',#14399);
#4343=VERTEX_POINT('',#14403);
#4344=VERTEX_POINT('',#14411);
#4345=VERTEX_POINT('',#14412);
#4346=VERTEX_POINT('',#14414);
#4347=VERTEX_POINT('',#14416);
#4348=VERTEX_POINT('',#14420);
#4349=VERTEX_POINT('',#14422);
#4350=VERTEX_POINT('',#14426);
#4351=VERTEX_POINT('',#14428);
#4352=VERTEX_POINT('',#14432);
#4353=VERTEX_POINT('',#14434);
#4354=VERTEX_POINT('',#14438);
#4355=VERTEX_POINT('',#14440);
#4356=VERTEX_POINT('',#14449);
#4357=VERTEX_POINT('',#14452);
#4358=VERTEX_POINT('',#14455);
#4359=VERTEX_POINT('',#14459);
#4360=VERTEX_POINT('',#14463);
#4361=VERTEX_POINT('',#14467);
#4362=VERTEX_POINT('',#14470);
#4363=VERTEX_POINT('',#14478);
#4364=VERTEX_POINT('',#14479);
#4365=VERTEX_POINT('',#14482);
#4366=VERTEX_POINT('',#14484);
#4367=VERTEX_POINT('',#14488);
#4368=VERTEX_POINT('',#14492);
#4369=VERTEX_POINT('',#14494);
#4370=VERTEX_POINT('',#14498);
#4371=VERTEX_POINT('',#14503);
#4372=VERTEX_POINT('',#14507);
#4373=VERTEX_POINT('',#14513);
#4374=VERTEX_POINT('',#14514);
#4375=VERTEX_POINT('',#14517);
#4376=VERTEX_POINT('',#14519);
#4377=VERTEX_POINT('',#14523);
#4378=VERTEX_POINT('',#14527);
#4379=VERTEX_POINT('',#14529);
#4380=VERTEX_POINT('',#14532);
#4381=VERTEX_POINT('',#14536);
#4382=VERTEX_POINT('',#14540);
#4383=VERTEX_POINT('',#14548);
#4384=VERTEX_POINT('',#14549);
#4385=VERTEX_POINT('',#14552);
#4386=VERTEX_POINT('',#14553);
#4387=VERTEX_POINT('',#14556);
#4388=VERTEX_POINT('',#14557);
#4389=VERTEX_POINT('',#14560);
#4390=VERTEX_POINT('',#14561);
#4391=VERTEX_POINT('',#14564);
#4392=VERTEX_POINT('',#14565);
#4393=VERTEX_POINT('',#14568);
#4394=VERTEX_POINT('',#14569);
#4395=VERTEX_POINT('',#14572);
#4396=VERTEX_POINT('',#14573);
#4397=VERTEX_POINT('',#14576);
#4398=VERTEX_POINT('',#14577);
#4399=VERTEX_POINT('',#14581);
#4400=VERTEX_POINT('',#14582);
#4401=VERTEX_POINT('',#14605);
#4402=VERTEX_POINT('',#14607);
#4403=VERTEX_POINT('',#14632);
#4404=VERTEX_POINT('',#14634);
#4405=VERTEX_POINT('',#14657);
#4406=VERTEX_POINT('',#14659);
#4407=VERTEX_POINT('',#14682);
#4408=VERTEX_POINT('',#14684);
#4409=VERTEX_POINT('',#14697);
#4410=VERTEX_POINT('',#14700);
#4411=VERTEX_POINT('',#14713);
#4412=VERTEX_POINT('',#14715);
#4413=VERTEX_POINT('',#14738);
#4414=VERTEX_POINT('',#14740);
#4415=VERTEX_POINT('',#14763);
#4416=VERTEX_POINT('',#14765);
#4417=VERTEX_POINT('',#14788);
#4418=VERTEX_POINT('',#14790);
#4419=VERTEX_POINT('',#14815);
#4420=VERTEX_POINT('',#14819);
#4421=VERTEX_POINT('',#14844);
#4422=VERTEX_POINT('',#14848);
#4423=VERTEX_POINT('',#14873);
#4424=VERTEX_POINT('',#14877);
#4425=VERTEX_POINT('',#14878);
#4426=VERTEX_POINT('',#14905);
#4427=VERTEX_POINT('',#14909);
#4428=VERTEX_POINT('',#14934);
#4429=VERTEX_POINT('',#14938);
#4430=VERTEX_POINT('',#14963);
#4431=VERTEX_POINT('',#14967);
#4432=VERTEX_POINT('',#14992);
#4433=VERTEX_POINT('',#14995);
#4434=VERTEX_POINT('',#14997);
#4435=VERTEX_POINT('',#15029);
#4436=VERTEX_POINT('',#15031);
#4437=VERTEX_POINT('',#15034);
#4438=VERTEX_POINT('',#15038);
#4439=VERTEX_POINT('',#15043);
#4440=VERTEX_POINT('',#15045);
#4441=VERTEX_POINT('',#15048);
#4442=VERTEX_POINT('',#15052);
#4443=VERTEX_POINT('',#15063);
#4444=VERTEX_POINT('',#15066);
#4445=VERTEX_POINT('',#15068);
#4446=VERTEX_POINT('',#15076);
#4447=VERTEX_POINT('',#15077);
#4448=VERTEX_POINT('',#15079);
#4449=VERTEX_POINT('',#15081);
#4450=VERTEX_POINT('',#15085);
#4451=VERTEX_POINT('',#15087);
#4452=VERTEX_POINT('',#15091);
#4453=VERTEX_POINT('',#15093);
#4454=VERTEX_POINT('',#15097);
#4455=VERTEX_POINT('',#15099);
#4456=VERTEX_POINT('',#15103);
#4457=VERTEX_POINT('',#15105);
#4458=VERTEX_POINT('',#15113);
#4459=VERTEX_POINT('',#15116);
#4460=VERTEX_POINT('',#15120);
#4461=VERTEX_POINT('',#15124);
#4462=VERTEX_POINT('',#15131);
#4463=VERTEX_POINT('',#15133);
#4464=VERTEX_POINT('',#15137);
#4465=VERTEX_POINT('',#15139);
#4466=VERTEX_POINT('',#15143);
#4467=VERTEX_POINT('',#15145);
#4468=VERTEX_POINT('',#15149);
#4469=VERTEX_POINT('',#15150);
#4470=VERTEX_POINT('',#15152);
#4471=VERTEX_POINT('',#15154);
#4472=VERTEX_POINT('',#15158);
#4473=VERTEX_POINT('',#15160);
#4474=VERTEX_POINT('',#15164);
#4475=VERTEX_POINT('',#15166);
#4476=VERTEX_POINT('',#15168);
#4477=VERTEX_POINT('',#15170);
#4478=VERTEX_POINT('',#15172);
#4479=VERTEX_POINT('',#15174);
#4480=VERTEX_POINT('',#15176);
#4481=VERTEX_POINT('',#15178);
#4482=VERTEX_POINT('',#15180);
#4483=VERTEX_POINT('',#15184);
#4484=VERTEX_POINT('',#15188);
#4485=VERTEX_POINT('',#15192);
#4486=VERTEX_POINT('',#15196);
#4487=VERTEX_POINT('',#15198);
#4488=VERTEX_POINT('',#15202);
#4489=VERTEX_POINT('',#15206);
#4490=VERTEX_POINT('',#15208);
#4491=VERTEX_POINT('',#15210);
#4492=VERTEX_POINT('',#15214);
#4493=VERTEX_POINT('',#15225);
#4494=VERTEX_POINT('',#15227);
#4495=VERTEX_POINT('',#15232);
#4496=VERTEX_POINT('',#15238);
#4497=VERTEX_POINT('',#15240);
#4498=VERTEX_POINT('',#15245);
#4499=VERTEX_POINT('',#15247);
#4500=VERTEX_POINT('',#15254);
#4501=VERTEX_POINT('',#15256);
#4502=VERTEX_POINT('',#15260);
#4503=VERTEX_POINT('',#15262);
#4504=VERTEX_POINT('',#15269);
#4505=VERTEX_POINT('',#15270);
#4506=VERTEX_POINT('',#15274);
#4507=VERTEX_POINT('',#15289);
#4508=VERTEX_POINT('',#15291);
#4509=VERTEX_POINT('',#15300);
#4510=VERTEX_POINT('',#15302);
#4511=VERTEX_POINT('',#15350);
#4512=VERTEX_POINT('',#15352);
#4513=VERTEX_POINT('',#15356);
#4514=VERTEX_POINT('',#15358);
#4515=VERTEX_POINT('',#15365);
#4516=VERTEX_POINT('',#15367);
#4517=VERTEX_POINT('',#15372);
#4518=VERTEX_POINT('',#15374);
#4519=VERTEX_POINT('',#15377);
#4520=VERTEX_POINT('',#15379);
#4521=VERTEX_POINT('',#15384);
#4522=VERTEX_POINT('',#15388);
#4523=VERTEX_POINT('',#15395);
#4524=VERTEX_POINT('',#15397);
#4525=VERTEX_POINT('',#15401);
#4526=VERTEX_POINT('',#15403);
#4527=VERTEX_POINT('',#15410);
#4528=VERTEX_POINT('',#15412);
#4529=VERTEX_POINT('',#15416);
#4530=VERTEX_POINT('',#15418);
#4531=VERTEX_POINT('',#15425);
#4532=VERTEX_POINT('',#15427);
#4533=VERTEX_POINT('',#15431);
#4534=VERTEX_POINT('',#15433);
#4535=VERTEX_POINT('',#15440);
#4536=VERTEX_POINT('',#15442);
#4537=VERTEX_POINT('',#15447);
#4538=VERTEX_POINT('',#15449);
#4539=VERTEX_POINT('',#15452);
#4540=VERTEX_POINT('',#15454);
#4541=VERTEX_POINT('',#15459);
#4542=VERTEX_POINT('',#15463);
#4543=VERTEX_POINT('',#15470);
#4544=VERTEX_POINT('',#15472);
#4545=VERTEX_POINT('',#15476);
#4546=VERTEX_POINT('',#15478);
#4547=VERTEX_POINT('',#15485);
#4548=VERTEX_POINT('',#15487);
#4549=VERTEX_POINT('',#15491);
#4550=VERTEX_POINT('',#15493);
#4551=VERTEX_POINT('',#15500);
#4552=VERTEX_POINT('',#15502);
#4553=VERTEX_POINT('',#15506);
#4554=VERTEX_POINT('',#15508);
#4555=VERTEX_POINT('',#15515);
#4556=VERTEX_POINT('',#15518);
#4557=VERTEX_POINT('',#15522);
#4558=VERTEX_POINT('',#15526);
#4559=VERTEX_POINT('',#15530);
#4560=VERTEX_POINT('',#15533);
#4561=VERTEX_POINT('',#15537);
#4562=VERTEX_POINT('',#15541);
#4563=VERTEX_POINT('',#15546);
#4564=VERTEX_POINT('',#15547);
#4565=VERTEX_POINT('',#15549);
#4566=VERTEX_POINT('',#15551);
#4567=VERTEX_POINT('',#15555);
#4568=VERTEX_POINT('',#15557);
#4569=VERTEX_POINT('',#15561);
#4570=VERTEX_POINT('',#15563);
#4571=VERTEX_POINT('',#15567);
#4572=VERTEX_POINT('',#15569);
#4573=VERTEX_POINT('',#15573);
#4574=VERTEX_POINT('',#15575);
#4575=VERTEX_POINT('',#15585);
#4576=VERTEX_POINT('',#15588);
#4577=VERTEX_POINT('',#15589);
#4578=VERTEX_POINT('',#15591);
#4579=VERTEX_POINT('',#15593);
#4580=VERTEX_POINT('',#15597);
#4581=VERTEX_POINT('',#15599);
#4582=VERTEX_POINT('',#15603);
#4583=VERTEX_POINT('',#15605);
#4584=VERTEX_POINT('',#15609);
#4585=VERTEX_POINT('',#15611);
#4586=VERTEX_POINT('',#15615);
#4587=VERTEX_POINT('',#15617);
#4588=VERTEX_POINT('',#15625);
#4589=VERTEX_POINT('',#15628);
#4590=VERTEX_POINT('',#15636);
#4591=VERTEX_POINT('',#15638);
#4592=VERTEX_POINT('',#15642);
#4593=VERTEX_POINT('',#15644);
#4594=VERTEX_POINT('',#15648);
#4595=VERTEX_POINT('',#15649);
#4596=VERTEX_POINT('',#15651);
#4597=VERTEX_POINT('',#15653);
#4598=VERTEX_POINT('',#15657);
#4599=VERTEX_POINT('',#15659);
#4600=VERTEX_POINT('',#15663);
#4601=VERTEX_POINT('',#15667);
#4602=VERTEX_POINT('',#15675);
#4603=VERTEX_POINT('',#15677);
#4604=VERTEX_POINT('',#15681);
#4605=VERTEX_POINT('',#15683);
#4606=VERTEX_POINT('',#15690);
#4607=VERTEX_POINT('',#15692);
#4608=VERTEX_POINT('',#15696);
#4609=VERTEX_POINT('',#15698);
#4610=VERTEX_POINT('',#15709);
#4611=VERTEX_POINT('',#15711);
#4612=VERTEX_POINT('',#15715);
#4613=VERTEX_POINT('',#15717);
#4614=VERTEX_POINT('',#15721);
#4615=VERTEX_POINT('',#15722);
#4616=VERTEX_POINT('',#15724);
#4617=VERTEX_POINT('',#15726);
#4618=VERTEX_POINT('',#15730);
#4619=VERTEX_POINT('',#15732);
#4620=VERTEX_POINT('',#15736);
#4621=VERTEX_POINT('',#15740);
#4622=VERTEX_POINT('',#15748);
#4623=VERTEX_POINT('',#15750);
#4624=VERTEX_POINT('',#15754);
#4625=VERTEX_POINT('',#15756);
#4626=VERTEX_POINT('',#15763);
#4627=VERTEX_POINT('',#15765);
#4628=VERTEX_POINT('',#15769);
#4629=VERTEX_POINT('',#15771);
#4630=VERTEX_POINT('',#15782);
#4631=VERTEX_POINT('',#15784);
#4632=VERTEX_POINT('',#15789);
#4633=VERTEX_POINT('',#15791);
#4634=VERTEX_POINT('',#15795);
#4635=VERTEX_POINT('',#15797);
#4636=VERTEX_POINT('',#15801);
#4637=VERTEX_POINT('',#15803);
#4638=VERTEX_POINT('',#15807);
#4639=VERTEX_POINT('',#15809);
#4640=VERTEX_POINT('',#15813);
#4641=VERTEX_POINT('',#15815);
#4642=VERTEX_POINT('',#15819);
#4643=VERTEX_POINT('',#15820);
#4644=VERTEX_POINT('',#15822);
#4645=VERTEX_POINT('',#15824);
#4646=VERTEX_POINT('',#15828);
#4647=VERTEX_POINT('',#15830);
#4648=VERTEX_POINT('',#15834);
#4649=VERTEX_POINT('',#15836);
#4650=VERTEX_POINT('',#15846);
#4651=VERTEX_POINT('',#15848);
#4652=VERTEX_POINT('',#15852);
#4653=VERTEX_POINT('',#15854);
#4654=VERTEX_POINT('',#15858);
#4655=VERTEX_POINT('',#15860);
#4656=VERTEX_POINT('',#15864);
#4657=VERTEX_POINT('',#15866);
#4658=VERTEX_POINT('',#15870);
#4659=VERTEX_POINT('',#15872);
#4660=VERTEX_POINT('',#15876);
#4661=VERTEX_POINT('',#15877);
#4662=VERTEX_POINT('',#15879);
#4663=VERTEX_POINT('',#15881);
#4664=VERTEX_POINT('',#15885);
#4665=VERTEX_POINT('',#15887);
#4666=VERTEX_POINT('',#15891);
#4667=VERTEX_POINT('',#15893);
#4668=VERTEX_POINT('',#15903);
#4669=VERTEX_POINT('',#15905);
#4670=VERTEX_POINT('',#15909);
#4671=VERTEX_POINT('',#15911);
#4672=VERTEX_POINT('',#15915);
#4673=VERTEX_POINT('',#15917);
#4674=VERTEX_POINT('',#15921);
#4675=VERTEX_POINT('',#15923);
#4676=VERTEX_POINT('',#15927);
#4677=VERTEX_POINT('',#15929);
#4678=VERTEX_POINT('',#15933);
#4679=VERTEX_POINT('',#15934);
#4680=VERTEX_POINT('',#15936);
#4681=VERTEX_POINT('',#15938);
#4682=VERTEX_POINT('',#15942);
#4683=VERTEX_POINT('',#15944);
#4684=VERTEX_POINT('',#15948);
#4685=VERTEX_POINT('',#15950);
#4686=VERTEX_POINT('',#15960);
#4687=VERTEX_POINT('',#15962);
#4688=VERTEX_POINT('',#15967);
#4689=VERTEX_POINT('',#15969);
#4690=VERTEX_POINT('',#15972);
#4691=VERTEX_POINT('',#15974);
#4692=VERTEX_POINT('',#15979);
#4693=VERTEX_POINT('',#15983);
#4694=VERTEX_POINT('',#15990);
#4695=VERTEX_POINT('',#15992);
#4696=VERTEX_POINT('',#15996);
#4697=VERTEX_POINT('',#15998);
#4698=VERTEX_POINT('',#16005);
#4699=VERTEX_POINT('',#16007);
#4700=VERTEX_POINT('',#16011);
#4701=VERTEX_POINT('',#16013);
#4702=VERTEX_POINT('',#16020);
#4703=VERTEX_POINT('',#16022);
#4704=VERTEX_POINT('',#16026);
#4705=VERTEX_POINT('',#16028);
#4706=VERTEX_POINT('',#16036);
#4707=VERTEX_POINT('',#16038);
#4708=VERTEX_POINT('',#16043);
#4709=VERTEX_POINT('',#16045);
#4710=VERTEX_POINT('',#16049);
#4711=VERTEX_POINT('',#16051);
#4712=VERTEX_POINT('',#16055);
#4713=VERTEX_POINT('',#16057);
#4714=VERTEX_POINT('',#16061);
#4715=VERTEX_POINT('',#16063);
#4716=VERTEX_POINT('',#16067);
#4717=VERTEX_POINT('',#16069);
#4718=VERTEX_POINT('',#16073);
#4719=VERTEX_POINT('',#16074);
#4720=VERTEX_POINT('',#16076);
#4721=VERTEX_POINT('',#16078);
#4722=VERTEX_POINT('',#16082);
#4723=VERTEX_POINT('',#16084);
#4724=VERTEX_POINT('',#16088);
#4725=VERTEX_POINT('',#16090);
#4726=VERTEX_POINT('',#16100);
#4727=VERTEX_POINT('',#16102);
#4728=VERTEX_POINT('',#16106);
#4729=VERTEX_POINT('',#16108);
#4730=VERTEX_POINT('',#16112);
#4731=VERTEX_POINT('',#16114);
#4732=VERTEX_POINT('',#16118);
#4733=VERTEX_POINT('',#16120);
#4734=VERTEX_POINT('',#16124);
#4735=VERTEX_POINT('',#16126);
#4736=VERTEX_POINT('',#16130);
#4737=VERTEX_POINT('',#16131);
#4738=VERTEX_POINT('',#16133);
#4739=VERTEX_POINT('',#16135);
#4740=VERTEX_POINT('',#16139);
#4741=VERTEX_POINT('',#16141);
#4742=VERTEX_POINT('',#16145);
#4743=VERTEX_POINT('',#16147);
#4744=VERTEX_POINT('',#16157);
#4745=VERTEX_POINT('',#16159);
#4746=VERTEX_POINT('',#16163);
#4747=VERTEX_POINT('',#16165);
#4748=VERTEX_POINT('',#16169);
#4749=VERTEX_POINT('',#16171);
#4750=VERTEX_POINT('',#16175);
#4751=VERTEX_POINT('',#16177);
#4752=VERTEX_POINT('',#16181);
#4753=VERTEX_POINT('',#16183);
#4754=VERTEX_POINT('',#16187);
#4755=VERTEX_POINT('',#16188);
#4756=VERTEX_POINT('',#16190);
#4757=VERTEX_POINT('',#16192);
#4758=VERTEX_POINT('',#16196);
#4759=VERTEX_POINT('',#16198);
#4760=VERTEX_POINT('',#16202);
#4761=VERTEX_POINT('',#16204);
#4762=VERTEX_POINT('',#16214);
#4763=VERTEX_POINT('',#16216);
#4764=VERTEX_POINT('',#16221);
#4765=VERTEX_POINT('',#16223);
#4766=VERTEX_POINT('',#16226);
#4767=VERTEX_POINT('',#16228);
#4768=VERTEX_POINT('',#16233);
#4769=VERTEX_POINT('',#16237);
#4770=VERTEX_POINT('',#16244);
#4771=VERTEX_POINT('',#16246);
#4772=VERTEX_POINT('',#16250);
#4773=VERTEX_POINT('',#16252);
#4774=VERTEX_POINT('',#16259);
#4775=VERTEX_POINT('',#16261);
#4776=VERTEX_POINT('',#16265);
#4777=VERTEX_POINT('',#16267);
#4778=VERTEX_POINT('',#16274);
#4779=VERTEX_POINT('',#16276);
#4780=VERTEX_POINT('',#16280);
#4781=VERTEX_POINT('',#16282);
#4782=VERTEX_POINT('',#16290);
#4783=VERTEX_POINT('',#16291);
#4784=VERTEX_POINT('',#16293);
#4785=VERTEX_POINT('',#16295);
#4786=VERTEX_POINT('',#16299);
#4787=VERTEX_POINT('',#16301);
#4788=VERTEX_POINT('',#16305);
#4789=VERTEX_POINT('',#16307);
#4790=VERTEX_POINT('',#16315);
#4791=VERTEX_POINT('',#16317);
#4792=VERTEX_POINT('',#16320);
#4793=VERTEX_POINT('',#16324);
#4794=VERTEX_POINT('',#16327);
#4795=VERTEX_POINT('',#16331);
#4796=VERTEX_POINT('',#16334);
#4797=VERTEX_POINT('',#16338);
#4798=VERTEX_POINT('',#16341);
#4799=VERTEX_POINT('',#16345);
#4800=VERTEX_POINT('',#16348);
#4801=VERTEX_POINT('',#16352);
#4802=VERTEX_POINT('',#16358);
#4803=VERTEX_POINT('',#16359);
#4804=VERTEX_POINT('',#16361);
#4805=VERTEX_POINT('',#16363);
#4806=VERTEX_POINT('',#16367);
#4807=VERTEX_POINT('',#16369);
#4808=VERTEX_POINT('',#16373);
#4809=VERTEX_POINT('',#16375);
#4810=VERTEX_POINT('',#16382);
#4811=VERTEX_POINT('',#16384);
#4812=VERTEX_POINT('',#16387);
#4813=VERTEX_POINT('',#16391);
#4814=VERTEX_POINT('',#16399);
#4815=VERTEX_POINT('',#16400);
#4816=VERTEX_POINT('',#16402);
#4817=VERTEX_POINT('',#16404);
#4818=VERTEX_POINT('',#16408);
#4819=VERTEX_POINT('',#16410);
#4820=VERTEX_POINT('',#16414);
#4821=VERTEX_POINT('',#16416);
#4822=VERTEX_POINT('',#16420);
#4823=VERTEX_POINT('',#16422);
#4824=VERTEX_POINT('',#16426);
#4825=VERTEX_POINT('',#16428);
#4826=VERTEX_POINT('',#16437);
#4827=VERTEX_POINT('',#16440);
#4828=VERTEX_POINT('',#16443);
#4829=VERTEX_POINT('',#16447);
#4830=VERTEX_POINT('',#16451);
#4831=VERTEX_POINT('',#16455);
#4832=VERTEX_POINT('',#16458);
#4833=EDGE_CURVE('',#4120,#4120,#3630,.T.);
#4834=EDGE_CURVE('',#4120,#4121,#2532,.T.);
#4835=EDGE_CURVE('',#4121,#4121,#3631,.T.);
#4836=EDGE_CURVE('',#4122,#4122,#3632,.T.);
#4837=EDGE_CURVE('',#4122,#4123,#2533,.T.);
#4838=EDGE_CURVE('',#4123,#4123,#3633,.T.);
#4839=EDGE_CURVE('',#4124,#4124,#3634,.T.);
#4840=EDGE_CURVE('',#4124,#4125,#2534,.T.);
#4841=EDGE_CURVE('',#4125,#4125,#3635,.T.);
#4842=EDGE_CURVE('',#4126,#4126,#3636,.T.);
#4843=EDGE_CURVE('',#4126,#4127,#2535,.T.);
#4844=EDGE_CURVE('',#4127,#4127,#3637,.T.);
#4845=EDGE_CURVE('',#4128,#4128,#3638,.T.);
#4846=EDGE_CURVE('',#4128,#4129,#2536,.T.);
#4847=EDGE_CURVE('',#4129,#4129,#3639,.T.);
#4848=EDGE_CURVE('',#4130,#4130,#3640,.T.);
#4849=EDGE_CURVE('',#4130,#4131,#2537,.T.);
#4850=EDGE_CURVE('',#4131,#4131,#3641,.T.);
#4851=EDGE_CURVE('',#4132,#4132,#3642,.T.);
#4852=EDGE_CURVE('',#4132,#4133,#2538,.T.);
#4853=EDGE_CURVE('',#4133,#4133,#3643,.T.);
#4854=EDGE_CURVE('',#4134,#4134,#3644,.T.);
#4855=EDGE_CURVE('',#4134,#4135,#2539,.T.);
#4856=EDGE_CURVE('',#4135,#4135,#3645,.T.);
#4857=EDGE_CURVE('',#4136,#4136,#3646,.T.);
#4858=EDGE_CURVE('',#4136,#4137,#2540,.T.);
#4859=EDGE_CURVE('',#4137,#4137,#3647,.T.);
#4860=EDGE_CURVE('',#4138,#4138,#3648,.T.);
#4861=EDGE_CURVE('',#4138,#4139,#2541,.T.);
#4862=EDGE_CURVE('',#4139,#4139,#3649,.T.);
#4863=EDGE_CURVE('',#4140,#4140,#3650,.T.);
#4864=EDGE_CURVE('',#4140,#4141,#2542,.T.);
#4865=EDGE_CURVE('',#4141,#4141,#3651,.T.);
#4866=EDGE_CURVE('',#4142,#4142,#3652,.T.);
#4867=EDGE_CURVE('',#4142,#4143,#2543,.T.);
#4868=EDGE_CURVE('',#4143,#4143,#3653,.T.);
#4869=EDGE_CURVE('',#4144,#4145,#2544,.T.);
#4870=EDGE_CURVE('',#4145,#4146,#2545,.T.);
#4871=EDGE_CURVE('',#4147,#4146,#2546,.T.);
#4872=EDGE_CURVE('',#4144,#4147,#2547,.T.);
#4873=EDGE_CURVE('',#4148,#4144,#2548,.T.);
#4874=EDGE_CURVE('',#4149,#4147,#2549,.T.);
#4875=EDGE_CURVE('',#4148,#4149,#2550,.T.);
#4876=EDGE_CURVE('',#4150,#4148,#2551,.T.);
#4877=EDGE_CURVE('',#4151,#4149,#2552,.T.);
#4878=EDGE_CURVE('',#4150,#4151,#2553,.T.);
#4879=EDGE_CURVE('',#4145,#4150,#2554,.T.);
#4880=EDGE_CURVE('',#4146,#4151,#2555,.T.);
#4881=EDGE_CURVE('',#4152,#4153,#2556,.T.);
#4882=EDGE_CURVE('',#4153,#4154,#2557,.T.);
#4883=EDGE_CURVE('',#4155,#4154,#2558,.T.);
#4884=EDGE_CURVE('',#4152,#4155,#2559,.T.);
#4885=EDGE_CURVE('',#4156,#4152,#2560,.T.);
#4886=EDGE_CURVE('',#4157,#4155,#2561,.T.);
#4887=EDGE_CURVE('',#4156,#4157,#2562,.T.);
#4888=EDGE_CURVE('',#4158,#4156,#2563,.T.);
#4889=EDGE_CURVE('',#4159,#4157,#2564,.T.);
#4890=EDGE_CURVE('',#4158,#4159,#2565,.T.);
#4891=EDGE_CURVE('',#4153,#4158,#2566,.T.);
#4892=EDGE_CURVE('',#4154,#4159,#2567,.T.);
#4893=EDGE_CURVE('',#4160,#4161,#2568,.T.);
#4894=EDGE_CURVE('',#4161,#4162,#2569,.T.);
#4895=EDGE_CURVE('',#4163,#4162,#2570,.T.);
#4896=EDGE_CURVE('',#4160,#4163,#2571,.T.);
#4897=EDGE_CURVE('',#4164,#4160,#2572,.T.);
#4898=EDGE_CURVE('',#4165,#4163,#2573,.T.);
#4899=EDGE_CURVE('',#4164,#4165,#2574,.T.);
#4900=EDGE_CURVE('',#4166,#4164,#2575,.T.);
#4901=EDGE_CURVE('',#4167,#4165,#2576,.T.);
#4902=EDGE_CURVE('',#4166,#4167,#2577,.T.);
#4903=EDGE_CURVE('',#4161,#4166,#2578,.T.);
#4904=EDGE_CURVE('',#4162,#4167,#2579,.T.);
#4905=EDGE_CURVE('',#4168,#4169,#457,.T.);
#4906=EDGE_CURVE('',#4169,#4168,#458,.T.);
#4907=EDGE_CURVE('',#4169,#4170,#2580,.T.);
#4908=EDGE_CURVE('',#4171,#4170,#459,.T.);
#4909=EDGE_CURVE('',#4170,#4171,#460,.T.);
#4910=EDGE_CURVE('',#4172,#4172,#3654,.T.);
#4911=EDGE_CURVE('',#4172,#4173,#2581,.T.);
#4912=EDGE_CURVE('',#4173,#4173,#3655,.T.);
#4913=EDGE_CURVE('',#4174,#4174,#3656,.T.);
#4914=EDGE_CURVE('',#4174,#4175,#2582,.T.);
#4915=EDGE_CURVE('',#4175,#4175,#3657,.T.);
#4916=EDGE_CURVE('',#4176,#4176,#3658,.T.);
#4917=EDGE_CURVE('',#4176,#4177,#2583,.T.);
#4918=EDGE_CURVE('',#4177,#4177,#3659,.T.);
#4919=EDGE_CURVE('',#4178,#4178,#3660,.T.);
#4920=EDGE_CURVE('',#4178,#4179,#2584,.T.);
#4921=EDGE_CURVE('',#4179,#4179,#3661,.T.);
#4922=EDGE_CURVE('',#4180,#4181,#3662,.T.);
#4923=EDGE_CURVE('',#4181,#4180,#3663,.T.);
#4924=EDGE_CURVE('',#4182,#4180,#2585,.T.);
#4925=EDGE_CURVE('',#4183,#4182,#3664,.T.);
#4926=EDGE_CURVE('',#4181,#4183,#2586,.T.);
#4927=EDGE_CURVE('',#4184,#4185,#2587,.T.);
#4928=EDGE_CURVE('',#4184,#4186,#3665,.T.);
#4929=EDGE_CURVE('',#4187,#4186,#2588,.T.);
#4930=EDGE_CURVE('',#4185,#4187,#3666,.T.);
#4931=EDGE_CURVE('',#4186,#4184,#3667,.T.);
#4932=EDGE_CURVE('',#4188,#4189,#2589,.T.);
#4933=EDGE_CURVE('',#4188,#4190,#3668,.T.);
#4934=EDGE_CURVE('',#4191,#4190,#2590,.T.);
#4935=EDGE_CURVE('',#4189,#4191,#3669,.T.);
#4936=EDGE_CURVE('',#4190,#4188,#3670,.T.);
#4937=EDGE_CURVE('',#4192,#4193,#2591,.T.);
#4938=EDGE_CURVE('',#4192,#4194,#3671,.T.);
#4939=EDGE_CURVE('',#4195,#4194,#2592,.T.);
#4940=EDGE_CURVE('',#4193,#4195,#3672,.T.);
#4941=EDGE_CURVE('',#4194,#4192,#3673,.T.);
#4942=EDGE_CURVE('',#4196,#4196,#3674,.T.);
#4943=EDGE_CURVE('',#4196,#4197,#2593,.T.);
#4944=EDGE_CURVE('',#4197,#4182,#3675,.T.);
#4945=EDGE_CURVE('',#4183,#4195,#3676,.T.);
#4946=EDGE_CURVE('',#4193,#4191,#3677,.T.);
#4947=EDGE_CURVE('',#4189,#4187,#3678,.T.);
#4948=EDGE_CURVE('',#4185,#4197,#3679,.T.);
#4949=EDGE_CURVE('',#4198,#4198,#3680,.T.);
#4950=EDGE_CURVE('',#4199,#4199,#3681,.T.);
#4951=EDGE_CURVE('',#4200,#4200,#3682,.T.);
#4952=EDGE_CURVE('',#4201,#4201,#3683,.T.);
#4953=EDGE_CURVE('',#4202,#4202,#3684,.T.);
#4954=EDGE_CURVE('',#4203,#4203,#3685,.T.);
#4955=EDGE_CURVE('',#4203,#4199,#2594,.T.);
#4956=EDGE_CURVE('',#4204,#4204,#3686,.T.);
#4957=EDGE_CURVE('',#4204,#4202,#2595,.T.);
#4958=EDGE_CURVE('',#4205,#4205,#3687,.T.);
#4959=EDGE_CURVE('',#4205,#4200,#2596,.T.);
#4960=EDGE_CURVE('',#4206,#4206,#3688,.T.);
#4961=EDGE_CURVE('',#4206,#4201,#2597,.T.);
#4962=EDGE_CURVE('',#4207,#4207,#3689,.T.);
#4963=EDGE_CURVE('',#4207,#4208,#2598,.T.);
#4964=EDGE_CURVE('',#4208,#4208,#3690,.T.);
#4965=EDGE_CURVE('',#4209,#4209,#3691,.T.);
#4966=EDGE_CURVE('',#4198,#4210,#2599,.T.);
#4967=EDGE_CURVE('',#4210,#4210,#3692,.T.);
#4968=EDGE_CURVE('',#4209,#4211,#2600,.T.);
#4969=EDGE_CURVE('',#4211,#4211,#3693,.T.);
#4970=EDGE_CURVE('',#4212,#4212,#3694,.T.);
#4971=EDGE_CURVE('',#4212,#4213,#2601,.T.);
#4972=EDGE_CURVE('',#4213,#4213,#3695,.T.);
#4973=EDGE_CURVE('',#4214,#4214,#3696,.T.);
#4974=EDGE_CURVE('',#4215,#4215,#3697,.T.);
#4975=EDGE_CURVE('',#4215,#4216,#2602,.T.);
#4976=EDGE_CURVE('',#4216,#4216,#3698,.T.);
#4977=EDGE_CURVE('',#4217,#4217,#3699,.T.);
#4978=EDGE_CURVE('',#4218,#4218,#3700,.T.);
#4979=EDGE_CURVE('',#4218,#4219,#2603,.T.);
#4980=EDGE_CURVE('',#4219,#4219,#3701,.T.);
#4981=EDGE_CURVE('',#4220,#4220,#3702,.T.);
#4982=EDGE_CURVE('',#4221,#4221,#3703,.T.);
#4983=EDGE_CURVE('',#4221,#4222,#2604,.T.);
#4984=EDGE_CURVE('',#4222,#4222,#3704,.T.);
#4985=EDGE_CURVE('',#4223,#4223,#3705,.T.);
#4986=EDGE_CURVE('',#4224,#4224,#3706,.T.);
#4987=EDGE_CURVE('',#4224,#4214,#2605,.T.);
#4988=EDGE_CURVE('',#4225,#4225,#3707,.T.);
#4989=EDGE_CURVE('',#4225,#4217,#2606,.T.);
#4990=EDGE_CURVE('',#4226,#4226,#3708,.T.);
#4991=EDGE_CURVE('',#4226,#4220,#2607,.T.);
#4992=EDGE_CURVE('',#4227,#4227,#3709,.T.);
#4993=EDGE_CURVE('',#4227,#4223,#2608,.T.);
#4994=EDGE_CURVE('',#4228,#4228,#3710,.T.);
#4995=EDGE_CURVE('',#4228,#4229,#2609,.T.);
#4996=EDGE_CURVE('',#4229,#4229,#3711,.T.);
#4997=EDGE_CURVE('',#4230,#4230,#3712,.T.);
#4998=EDGE_CURVE('',#4231,#4231,#3713,.T.);
#4999=EDGE_CURVE('',#4231,#4230,#2610,.T.);
#5000=EDGE_CURVE('',#4232,#4232,#3714,.T.);
#5001=EDGE_CURVE('',#4232,#4233,#2611,.T.);
#5002=EDGE_CURVE('',#4233,#4233,#3715,.T.);
#5003=EDGE_CURVE('',#4234,#4235,#2612,.T.);
#5004=EDGE_CURVE('',#4236,#4234,#3716,.T.);
#5005=EDGE_CURVE('',#4236,#4237,#2613,.T.);
#5006=EDGE_CURVE('',#4235,#4237,#3717,.T.);
#5007=EDGE_CURVE('',#4238,#4239,#2614,.T.);
#5008=EDGE_CURVE('',#4240,#4238,#3718,.T.);
#5009=EDGE_CURVE('',#4240,#4241,#2615,.T.);
#5010=EDGE_CURVE('',#4239,#4241,#3719,.T.);
#5011=EDGE_CURVE('',#4242,#4243,#2616,.T.);
#5012=EDGE_CURVE('',#4242,#4243,#3720,.T.);
#5013=EDGE_CURVE('',#4244,#4245,#461,.T.);
#5014=EDGE_CURVE('',#4246,#4244,#3721,.T.);
#5015=EDGE_CURVE('',#4247,#4246,#462,.T.);
#5016=EDGE_CURVE('',#4243,#4247,#463,.T.);
#5017=EDGE_CURVE('',#4245,#4242,#464,.T.);
#5018=EDGE_CURVE('',#4245,#4248,#2617,.T.);
#5019=EDGE_CURVE('',#4248,#4248,#3722,.T.);
#5020=EDGE_CURVE('',#4246,#4244,#2618,.T.);
#5021=EDGE_CURVE('',#4241,#4239,#3723,.T.);
#5022=EDGE_CURVE('',#4240,#4241,#2619,.T.);
#5023=EDGE_CURVE('',#4238,#4240,#3724,.T.);
#5024=EDGE_CURVE('',#4249,#4249,#3725,.T.);
#5025=EDGE_CURVE('',#4237,#4235,#3726,.T.);
#5026=EDGE_CURVE('',#4236,#4237,#2620,.T.);
#5027=EDGE_CURVE('',#4234,#4236,#3727,.T.);
#5028=EDGE_CURVE('',#4250,#4250,#3728,.T.);
#5029=EDGE_CURVE('',#4251,#4252,#2621,.T.);
#5030=EDGE_CURVE('',#4252,#4241,#2622,.T.);
#5031=EDGE_CURVE('',#4241,#4253,#2623,.T.);
#5032=EDGE_CURVE('',#4253,#4254,#2624,.T.);
#5033=EDGE_CURVE('',#4254,#4237,#2625,.T.);
#5034=EDGE_CURVE('',#4237,#4251,#2626,.T.);
#5035=EDGE_CURVE('',#4255,#4255,#3729,.T.);
#5036=EDGE_CURVE('',#4255,#4249,#2627,.T.);
#5037=EDGE_CURVE('',#4256,#4256,#3730,.T.);
#5038=EDGE_CURVE('',#4256,#4250,#2628,.T.);
#5039=EDGE_CURVE('',#4257,#4257,#3731,.T.);
#5040=EDGE_CURVE('',#4257,#4245,#2629,.T.);
#5041=EDGE_CURVE('',#4247,#4258,#2630,.T.);
#5042=EDGE_CURVE('',#4258,#4258,#3732,.T.);
#5043=EDGE_CURVE('',#4259,#4260,#2631,.T.);
#5044=EDGE_CURVE('',#4260,#4251,#2632,.T.);
#5045=EDGE_CURVE('',#4259,#4254,#2633,.T.);
#5046=EDGE_CURVE('',#4261,#4259,#2634,.T.);
#5047=EDGE_CURVE('',#4261,#4253,#2635,.T.);
#5048=EDGE_CURVE('',#4262,#4261,#2636,.T.);
#5049=EDGE_CURVE('',#4262,#4252,#2637,.T.);
#5050=EDGE_CURVE('',#4260,#4262,#2638,.T.);
#5051=EDGE_CURVE('',#4263,#4264,#2639,.T.);
#5052=EDGE_CURVE('',#4265,#4263,#3733,.T.);
#5053=EDGE_CURVE('',#4265,#4266,#2640,.T.);
#5054=EDGE_CURVE('',#4264,#4266,#3734,.T.);
#5055=EDGE_CURVE('',#4267,#4268,#2641,.T.);
#5056=EDGE_CURVE('',#4269,#4267,#3735,.T.);
#5057=EDGE_CURVE('',#4269,#4270,#2642,.T.);
#5058=EDGE_CURVE('',#4268,#4270,#3736,.T.);
#5059=EDGE_CURVE('',#4271,#4272,#2643,.T.);
#5060=EDGE_CURVE('',#4271,#4272,#3737,.T.);
#5061=EDGE_CURVE('',#4273,#4274,#465,.T.);
#5062=EDGE_CURVE('',#4275,#4273,#3738,.T.);
#5063=EDGE_CURVE('',#4276,#4275,#466,.T.);
#5064=EDGE_CURVE('',#4272,#4276,#467,.T.);
#5065=EDGE_CURVE('',#4274,#4271,#468,.T.);
#5066=EDGE_CURVE('',#4274,#4277,#2644,.T.);
#5067=EDGE_CURVE('',#4277,#4277,#3739,.T.);
#5068=EDGE_CURVE('',#4275,#4273,#2645,.T.);
#5069=EDGE_CURVE('',#4270,#4268,#3740,.T.);
#5070=EDGE_CURVE('',#4269,#4270,#2646,.T.);
#5071=EDGE_CURVE('',#4267,#4269,#3741,.T.);
#5072=EDGE_CURVE('',#4278,#4278,#3742,.T.);
#5073=EDGE_CURVE('',#4266,#4264,#3743,.T.);
#5074=EDGE_CURVE('',#4265,#4266,#2647,.T.);
#5075=EDGE_CURVE('',#4263,#4265,#3744,.T.);
#5076=EDGE_CURVE('',#4279,#4279,#3745,.T.);
#5077=EDGE_CURVE('',#4280,#4281,#2648,.T.);
#5078=EDGE_CURVE('',#4281,#4270,#2649,.T.);
#5079=EDGE_CURVE('',#4270,#4282,#2650,.T.);
#5080=EDGE_CURVE('',#4282,#4283,#2651,.T.);
#5081=EDGE_CURVE('',#4283,#4266,#2652,.T.);
#5082=EDGE_CURVE('',#4266,#4280,#2653,.T.);
#5083=EDGE_CURVE('',#4284,#4284,#3746,.T.);
#5084=EDGE_CURVE('',#4284,#4278,#2654,.T.);
#5085=EDGE_CURVE('',#4285,#4285,#3747,.T.);
#5086=EDGE_CURVE('',#4285,#4279,#2655,.T.);
#5087=EDGE_CURVE('',#4286,#4286,#3748,.T.);
#5088=EDGE_CURVE('',#4286,#4274,#2656,.T.);
#5089=EDGE_CURVE('',#4276,#4287,#2657,.T.);
#5090=EDGE_CURVE('',#4287,#4287,#3749,.T.);
#5091=EDGE_CURVE('',#4288,#4289,#2658,.T.);
#5092=EDGE_CURVE('',#4289,#4280,#2659,.T.);
#5093=EDGE_CURVE('',#4288,#4283,#2660,.T.);
#5094=EDGE_CURVE('',#4290,#4288,#2661,.T.);
#5095=EDGE_CURVE('',#4290,#4282,#2662,.T.);
#5096=EDGE_CURVE('',#4291,#4290,#2663,.T.);
#5097=EDGE_CURVE('',#4291,#4281,#2664,.T.);
#5098=EDGE_CURVE('',#4289,#4291,#2665,.T.);
#5099=EDGE_CURVE('',#4292,#4293,#2666,.T.);
#5100=EDGE_CURVE('',#4294,#4292,#3750,.T.);
#5101=EDGE_CURVE('',#4294,#4295,#2667,.T.);
#5102=EDGE_CURVE('',#4293,#4295,#3751,.T.);
#5103=EDGE_CURVE('',#4296,#4297,#2668,.T.);
#5104=EDGE_CURVE('',#4296,#4297,#3752,.T.);
#5105=EDGE_CURVE('',#4298,#4296,#469,.T.);
#5106=EDGE_CURVE('',#4299,#4298,#3753,.T.);
#5107=EDGE_CURVE('',#4299,#4300,#2669,.T.);
#5108=EDGE_CURVE('',#4300,#4300,#3754,.T.);
#5109=EDGE_CURVE('',#4301,#4299,#3755,.T.);
#5110=EDGE_CURVE('',#4297,#4301,#470,.T.);
#5111=EDGE_CURVE('',#4301,#4298,#2670,.T.);
#5112=EDGE_CURVE('',#4302,#4302,#3756,.T.);
#5113=EDGE_CURVE('',#4302,#4303,#2671,.T.);
#5114=EDGE_CURVE('',#4303,#4303,#3757,.T.);
#5115=EDGE_CURVE('',#4302,#4303,#2672,.T.);
#5116=EDGE_CURVE('',#4304,#4304,#3758,.T.);
#5117=EDGE_CURVE('',#4295,#4293,#3759,.T.);
#5118=EDGE_CURVE('',#4294,#4295,#2673,.T.);
#5119=EDGE_CURVE('',#4292,#4294,#3760,.T.);
#5120=EDGE_CURVE('',#4305,#4305,#3761,.T.);
#5121=EDGE_CURVE('',#4306,#4303,#2674,.T.);
#5122=EDGE_CURVE('',#4303,#4307,#2675,.T.);
#5123=EDGE_CURVE('',#4307,#4308,#2676,.T.);
#5124=EDGE_CURVE('',#4308,#4295,#2677,.T.);
#5125=EDGE_CURVE('',#4295,#4309,#2678,.T.);
#5126=EDGE_CURVE('',#4309,#4306,#2679,.T.);
#5127=EDGE_CURVE('',#4310,#4310,#3762,.T.);
#5128=EDGE_CURVE('',#4310,#4304,#2680,.T.);
#5129=EDGE_CURVE('',#4311,#4311,#3763,.T.);
#5130=EDGE_CURVE('',#4311,#4305,#2681,.T.);
#5131=EDGE_CURVE('',#4312,#4312,#3764,.T.);
#5132=EDGE_CURVE('',#4312,#4313,#2682,.T.);
#5133=EDGE_CURVE('',#4313,#4313,#3765,.T.);
#5134=EDGE_CURVE('',#4314,#4315,#2683,.T.);
#5135=EDGE_CURVE('',#4315,#4306,#2684,.T.);
#5136=EDGE_CURVE('',#4314,#4309,#2685,.T.);
#5137=EDGE_CURVE('',#4316,#4314,#2686,.T.);
#5138=EDGE_CURVE('',#4316,#4308,#2687,.T.);
#5139=EDGE_CURVE('',#4317,#4316,#2688,.T.);
#5140=EDGE_CURVE('',#4317,#4307,#2689,.T.);
#5141=EDGE_CURVE('',#4315,#4317,#2690,.T.);
#5142=EDGE_CURVE('',#4318,#4319,#2691,.T.);
#5143=EDGE_CURVE('',#4320,#4318,#3766,.T.);
#5144=EDGE_CURVE('',#4320,#4321,#2692,.T.);
#5145=EDGE_CURVE('',#4319,#4321,#3767,.T.);
#5146=EDGE_CURVE('',#4322,#4323,#2693,.T.);
#5147=EDGE_CURVE('',#4322,#4323,#3768,.T.);
#5148=EDGE_CURVE('',#4324,#4322,#471,.T.);
#5149=EDGE_CURVE('',#4325,#4324,#3769,.T.);
#5150=EDGE_CURVE('',#4325,#4326,#2694,.T.);
#5151=EDGE_CURVE('',#4326,#4326,#3770,.T.);
#5152=EDGE_CURVE('',#4327,#4325,#3771,.T.);
#5153=EDGE_CURVE('',#4323,#4327,#472,.T.);
#5154=EDGE_CURVE('',#4327,#4324,#2695,.T.);
#5155=EDGE_CURVE('',#4328,#4328,#3772,.T.);
#5156=EDGE_CURVE('',#4328,#4329,#2696,.T.);
#5157=EDGE_CURVE('',#4329,#4329,#3773,.T.);
#5158=EDGE_CURVE('',#4328,#4329,#2697,.T.);
#5159=EDGE_CURVE('',#4330,#4330,#3774,.T.);
#5160=EDGE_CURVE('',#4321,#4319,#3775,.T.);
#5161=EDGE_CURVE('',#4320,#4321,#2698,.T.);
#5162=EDGE_CURVE('',#4318,#4320,#3776,.T.);
#5163=EDGE_CURVE('',#4331,#4331,#3777,.T.);
#5164=EDGE_CURVE('',#4332,#4329,#2699,.T.);
#5165=EDGE_CURVE('',#4329,#4333,#2700,.T.);
#5166=EDGE_CURVE('',#4333,#4334,#2701,.T.);
#5167=EDGE_CURVE('',#4334,#4321,#2702,.T.);
#5168=EDGE_CURVE('',#4321,#4335,#2703,.T.);
#5169=EDGE_CURVE('',#4335,#4332,#2704,.T.);
#5170=EDGE_CURVE('',#4336,#4336,#3778,.T.);
#5171=EDGE_CURVE('',#4336,#4330,#2705,.T.);
#5172=EDGE_CURVE('',#4337,#4337,#3779,.T.);
#5173=EDGE_CURVE('',#4337,#4331,#2706,.T.);
#5174=EDGE_CURVE('',#4338,#4338,#3780,.T.);
#5175=EDGE_CURVE('',#4338,#4339,#2707,.T.);
#5176=EDGE_CURVE('',#4339,#4339,#3781,.T.);
#5177=EDGE_CURVE('',#4340,#4341,#2708,.T.);
#5178=EDGE_CURVE('',#4341,#4332,#2709,.T.);
#5179=EDGE_CURVE('',#4340,#4335,#2710,.T.);
#5180=EDGE_CURVE('',#4342,#4340,#2711,.T.);
#5181=EDGE_CURVE('',#4342,#4334,#2712,.T.);
#5182=EDGE_CURVE('',#4343,#4342,#2713,.T.);
#5183=EDGE_CURVE('',#4343,#4333,#2714,.T.);
#5184=EDGE_CURVE('',#4341,#4343,#2715,.T.);
#5185=EDGE_CURVE('',#4344,#4345,#2716,.T.);
#5186=EDGE_CURVE('',#4345,#4346,#2717,.T.);
#5187=EDGE_CURVE('',#4346,#4347,#2718,.T.);
#5188=EDGE_CURVE('',#4344,#4347,#2719,.T.);
#5189=EDGE_CURVE('',#4345,#4348,#2720,.T.);
#5190=EDGE_CURVE('',#4348,#4349,#2721,.T.);
#5191=EDGE_CURVE('',#4349,#4346,#2722,.T.);
#5192=EDGE_CURVE('',#4348,#4350,#2723,.T.);
#5193=EDGE_CURVE('',#4350,#4351,#2724,.T.);
#5194=EDGE_CURVE('',#4351,#4349,#2725,.T.);
#5195=EDGE_CURVE('',#4350,#4352,#2726,.T.);
#5196=EDGE_CURVE('',#4352,#4353,#2727,.T.);
#5197=EDGE_CURVE('',#4353,#4351,#2728,.T.);
#5198=EDGE_CURVE('',#4352,#4354,#2729,.T.);
#5199=EDGE_CURVE('',#4354,#4355,#2730,.T.);
#5200=EDGE_CURVE('',#4355,#4353,#2731,.T.);
#5201=EDGE_CURVE('',#4354,#4344,#2732,.T.);
#5202=EDGE_CURVE('',#4347,#4355,#2733,.T.);
#5203=EDGE_CURVE('',#4356,#4356,#3782,.T.);
#5204=EDGE_CURVE('',#4357,#4357,#3783,.T.);
#5205=EDGE_CURVE('',#4358,#4358,#3784,.T.);
#5206=EDGE_CURVE('',#4358,#4357,#2734,.T.);
#5207=EDGE_CURVE('',#4359,#4359,#3785,.T.);
#5208=EDGE_CURVE('',#4359,#4358,#2735,.T.);
#5209=EDGE_CURVE('',#4360,#4360,#3786,.T.);
#5210=EDGE_CURVE('',#4360,#4359,#2736,.T.);
#5211=EDGE_CURVE('',#4361,#4361,#3787,.T.);
#5212=EDGE_CURVE('',#4362,#4362,#3788,.F.);
#5213=EDGE_CURVE('',#4362,#4361,#2737,.T.);
#5214=EDGE_CURVE('',#4356,#4362,#2738,.T.);
#5215=EDGE_CURVE('',#4363,#4364,#3789,.T.);
#5216=EDGE_CURVE('',#4364,#4363,#3790,.T.);
#5217=EDGE_CURVE('',#4364,#4365,#3791,.T.);
#5218=EDGE_CURVE('',#4366,#4365,#3792,.T.);
#5219=EDGE_CURVE('',#4365,#4366,#3793,.T.);
#5220=EDGE_CURVE('',#4366,#4367,#2739,.T.);
#5221=EDGE_CURVE('',#4367,#4367,#3794,.T.);
#5222=EDGE_CURVE('',#4368,#4368,#3795,.T.);
#5223=EDGE_CURVE('',#4368,#4369,#2740,.T.);
#5224=EDGE_CURVE('',#4369,#4369,#3796,.T.);
#5225=EDGE_CURVE('',#4369,#4370,#2741,.T.);
#5226=EDGE_CURVE('',#4370,#4370,#3797,.T.);
#5227=EDGE_CURVE('',#4371,#4371,#3798,.T.);
#5228=EDGE_CURVE('',#4371,#4363,#2742,.T.);
#5229=EDGE_CURVE('',#4372,#4372,#3799,.T.);
#5230=EDGE_CURVE('',#4372,#4368,#2743,.T.);
#5231=EDGE_CURVE('',#4373,#4374,#3800,.T.);
#5232=EDGE_CURVE('',#4374,#4373,#3801,.T.);
#5233=EDGE_CURVE('',#4374,#4375,#3802,.T.);
#5234=EDGE_CURVE('',#4376,#4375,#3803,.T.);
#5235=EDGE_CURVE('',#4375,#4376,#3804,.T.);
#5236=EDGE_CURVE('',#4377,#4377,#3805,.T.);
#5237=EDGE_CURVE('',#4377,#4376,#2744,.T.);
#5238=EDGE_CURVE('',#4378,#4378,#3806,.T.);
#5239=EDGE_CURVE('',#4379,#4379,#3807,.T.);
#5240=EDGE_CURVE('',#4380,#4380,#3808,.T.);
#5241=EDGE_CURVE('',#4380,#4378,#2745,.T.);
#5242=EDGE_CURVE('',#4381,#4381,#3809,.T.);
#5243=EDGE_CURVE('',#4381,#4380,#2746,.T.);
#5244=EDGE_CURVE('',#4382,#4382,#3810,.T.);
#5245=EDGE_CURVE('',#4382,#4381,#2747,.T.);
#5246=EDGE_CURVE('',#4373,#4379,#2748,.T.);
#5247=EDGE_CURVE('',#4383,#4384,#3811,.T.);
#5248=EDGE_CURVE('',#4385,#4386,#3812,.T.);
#5249=EDGE_CURVE('',#4387,#4388,#3813,.T.);
#5250=EDGE_CURVE('',#4389,#4390,#3814,.T.);
#5251=EDGE_CURVE('',#4391,#4392,#3815,.T.);
#5252=EDGE_CURVE('',#4393,#4394,#3816,.T.);
#5253=EDGE_CURVE('',#4395,#4396,#3817,.T.);
#5254=EDGE_CURVE('',#4397,#4398,#3818,.T.);
#5255=EDGE_CURVE('',#4399,#4400,#473,.T.);
#5256=EDGE_CURVE('',#4401,#4399,#3819,.T.);
#5257=EDGE_CURVE('',#4402,#4401,#474,.T.);
#5258=EDGE_CURVE('',#4400,#4402,#3820,.T.);
#5259=EDGE_CURVE('',#4403,#4401,#3821,.T.);
#5260=EDGE_CURVE('',#4403,#4404,#475,.T.);
#5261=EDGE_CURVE('',#4405,#4404,#3822,.T.);
#5262=EDGE_CURVE('',#4405,#4406,#476,.T.);
#5263=EDGE_CURVE('',#4407,#4406,#3823,.T.);
#5264=EDGE_CURVE('',#4407,#4408,#477,.T.);
#5265=EDGE_CURVE('',#4408,#4409,#2749,.T.);
#5266=EDGE_CURVE('',#4409,#4409,#3824,.T.);
#5267=EDGE_CURVE('',#4408,#4410,#478,.T.);
#5268=EDGE_CURVE('',#4411,#4410,#3825,.T.);
#5269=EDGE_CURVE('',#4411,#4412,#479,.T.);
#5270=EDGE_CURVE('',#4413,#4412,#3826,.T.);
#5271=EDGE_CURVE('',#4413,#4414,#480,.T.);
#5272=EDGE_CURVE('',#4415,#4414,#3827,.T.);
#5273=EDGE_CURVE('',#4415,#4416,#481,.T.);
#5274=EDGE_CURVE('',#4417,#4416,#3828,.T.);
#5275=EDGE_CURVE('',#4417,#4418,#482,.T.);
#5276=EDGE_CURVE('',#4402,#4418,#3829,.T.);
#5277=EDGE_CURVE('',#4399,#4419,#3830,.T.);
#5278=EDGE_CURVE('',#4419,#4403,#3831,.T.);
#5279=EDGE_CURVE('',#4420,#4419,#483,.T.);
#5280=EDGE_CURVE('',#4404,#4420,#3832,.T.);
#5281=EDGE_CURVE('',#4420,#4421,#3833,.T.);
#5282=EDGE_CURVE('',#4421,#4405,#3834,.T.);
#5283=EDGE_CURVE('',#4422,#4421,#484,.T.);
#5284=EDGE_CURVE('',#4406,#4422,#3835,.T.);
#5285=EDGE_CURVE('',#4422,#4423,#3836,.T.);
#5286=EDGE_CURVE('',#4423,#4407,#3837,.T.);
#5287=EDGE_CURVE('',#4424,#4425,#485,.T.);
#5288=EDGE_CURVE('',#4410,#4424,#3838,.T.);
#5289=EDGE_CURVE('',#4425,#4423,#486,.T.);
#5290=EDGE_CURVE('',#4424,#4426,#3839,.T.);
#5291=EDGE_CURVE('',#4426,#4411,#3840,.T.);
#5292=EDGE_CURVE('',#4427,#4426,#487,.T.);
#5293=EDGE_CURVE('',#4412,#4427,#3841,.T.);
#5294=EDGE_CURVE('',#4427,#4428,#3842,.T.);
#5295=EDGE_CURVE('',#4428,#4413,#3843,.T.);
#5296=EDGE_CURVE('',#4429,#4428,#488,.T.);
#5297=EDGE_CURVE('',#4414,#4429,#3844,.T.);
#5298=EDGE_CURVE('',#4429,#4430,#3845,.T.);
#5299=EDGE_CURVE('',#4430,#4415,#3846,.T.);
#5300=EDGE_CURVE('',#4431,#4430,#489,.T.);
#5301=EDGE_CURVE('',#4416,#4431,#3847,.T.);
#5302=EDGE_CURVE('',#4432,#4432,#3848,.T.);
#5303=EDGE_CURVE('',#4432,#4425,#2750,.T.);
#5304=EDGE_CURVE('',#4433,#4400,#3849,.T.);
#5305=EDGE_CURVE('',#4433,#4434,#490,.T.);
#5306=EDGE_CURVE('',#4431,#4434,#3850,.T.);
#5307=EDGE_CURVE('',#4418,#4433,#3851,.T.);
#5308=EDGE_CURVE('',#4434,#4417,#3852,.T.);
#5309=EDGE_CURVE('',#4435,#4435,#3853,.T.);
#5310=EDGE_CURVE('',#4436,#4436,#3854,.T.);
#5311=EDGE_CURVE('',#4437,#4437,#3855,.T.);
#5312=EDGE_CURVE('',#4437,#4435,#2751,.T.);
#5313=EDGE_CURVE('',#4438,#4438,#3856,.T.);
#5314=EDGE_CURVE('',#4438,#4436,#2752,.T.);
#5315=EDGE_CURVE('',#4439,#4439,#3857,.T.);
#5316=EDGE_CURVE('',#4440,#4440,#3858,.T.);
#5317=EDGE_CURVE('',#4441,#4441,#3859,.T.);
#5318=EDGE_CURVE('',#4441,#4439,#2753,.T.);
#5319=EDGE_CURVE('',#4442,#4442,#3860,.T.);
#5320=EDGE_CURVE('',#4442,#4440,#2754,.T.);
#5321=EDGE_CURVE('',#4443,#4443,#3861,.T.);
#5322=EDGE_CURVE('',#4444,#4444,#3862,.T.);
#5323=EDGE_CURVE('',#4444,#4445,#2755,.T.);
#5324=EDGE_CURVE('',#4445,#4445,#3863,.T.);
#5325=EDGE_CURVE('',#4443,#4444,#2756,.T.);
#5326=EDGE_CURVE('',#4446,#4447,#2757,.T.);
#5327=EDGE_CURVE('',#4446,#4448,#2758,.T.);
#5328=EDGE_CURVE('',#4448,#4449,#2759,.T.);
#5329=EDGE_CURVE('',#4447,#4449,#2760,.T.);
#5330=EDGE_CURVE('',#4450,#4446,#2761,.T.);
#5331=EDGE_CURVE('',#4450,#4451,#2762,.T.);
#5332=EDGE_CURVE('',#4451,#4448,#2763,.T.);
#5333=EDGE_CURVE('',#4452,#4450,#2764,.T.);
#5334=EDGE_CURVE('',#4452,#4453,#2765,.T.);
#5335=EDGE_CURVE('',#4453,#4451,#2766,.T.);
#5336=EDGE_CURVE('',#4454,#4452,#2767,.T.);
#5337=EDGE_CURVE('',#4454,#4455,#2768,.T.);
#5338=EDGE_CURVE('',#4455,#4453,#2769,.T.);
#5339=EDGE_CURVE('',#4456,#4454,#2770,.T.);
#5340=EDGE_CURVE('',#4456,#4457,#2771,.T.);
#5341=EDGE_CURVE('',#4457,#4455,#2772,.T.);
#5342=EDGE_CURVE('',#4447,#4456,#2773,.T.);
#5343=EDGE_CURVE('',#4449,#4457,#2774,.T.);
#5344=EDGE_CURVE('',#4458,#4458,#3864,.T.);
#5345=EDGE_CURVE('',#4459,#4459,#3865,.T.);
#5346=EDGE_CURVE('',#4459,#4458,#2775,.T.);
#5347=EDGE_CURVE('',#4460,#4460,#3866,.F.);
#5348=EDGE_CURVE('',#4460,#4459,#2776,.T.);
#5349=EDGE_CURVE('',#4461,#4461,#3867,.T.);
#5350=EDGE_CURVE('',#4461,#4460,#2777,.T.);
#5351=EDGE_CURVE('',#4462,#4462,#3868,.T.);
#5352=EDGE_CURVE('',#4462,#4463,#2778,.T.);
#5353=EDGE_CURVE('',#4463,#4463,#3869,.T.);
#5354=EDGE_CURVE('',#4464,#4464,#3870,.T.);
#5355=EDGE_CURVE('',#4464,#4465,#2779,.T.);
#5356=EDGE_CURVE('',#4465,#4465,#3871,.T.);
#5357=EDGE_CURVE('',#4466,#4466,#3872,.T.);
#5358=EDGE_CURVE('',#4466,#4467,#2780,.T.);
#5359=EDGE_CURVE('',#4467,#4467,#3873,.T.);
#5360=EDGE_CURVE('',#4468,#4469,#2781,.T.);
#5361=EDGE_CURVE('',#4468,#4470,#3874,.T.);
#5362=EDGE_CURVE('',#4471,#4470,#2782,.T.);
#5363=EDGE_CURVE('',#4469,#4471,#3875,.T.);
#5364=EDGE_CURVE('',#4472,#4469,#2783,.T.);
#5365=EDGE_CURVE('',#4473,#4472,#2784,.T.);
#5366=EDGE_CURVE('',#4468,#4473,#2785,.T.);
#5367=EDGE_CURVE('',#4471,#4474,#2786,.T.);
#5368=EDGE_CURVE('',#4474,#4475,#3876,.T.);
#5369=EDGE_CURVE('',#4475,#4476,#2787,.T.);
#5370=EDGE_CURVE('',#4476,#4477,#3877,.T.);
#5371=EDGE_CURVE('',#4477,#4478,#2788,.T.);
#5372=EDGE_CURVE('',#4478,#4479,#3878,.T.);
#5373=EDGE_CURVE('',#4479,#4480,#2789,.T.);
#5374=EDGE_CURVE('',#4480,#4481,#3879,.T.);
#5375=EDGE_CURVE('',#4481,#4482,#2790,.T.);
#5376=EDGE_CURVE('',#4482,#4472,#3880,.T.);
#5377=EDGE_CURVE('',#4483,#4470,#2791,.T.);
#5378=EDGE_CURVE('',#4474,#4483,#2792,.T.);
#5379=EDGE_CURVE('',#4482,#4484,#2793,.T.);
#5380=EDGE_CURVE('',#4484,#4473,#3881,.T.);
#5381=EDGE_CURVE('',#4483,#4485,#3882,.T.);
#5382=EDGE_CURVE('',#4485,#4475,#2794,.T.);
#5383=EDGE_CURVE('',#4477,#4486,#2795,.T.);
#5384=EDGE_CURVE('',#4487,#4476,#2796,.T.);
#5385=EDGE_CURVE('',#4487,#4486,#3883,.T.);
#5386=EDGE_CURVE('',#4488,#4486,#2797,.T.);
#5387=EDGE_CURVE('',#4478,#4488,#2798,.T.);
#5388=EDGE_CURVE('',#4484,#4489,#2799,.T.);
#5389=EDGE_CURVE('',#4490,#4489,#3884,.T.);
#5390=EDGE_CURVE('',#4490,#4491,#2800,.T.);
#5391=EDGE_CURVE('',#4488,#4491,#3885,.T.);
#5392=EDGE_CURVE('',#4487,#4485,#2801,.T.);
#5393=EDGE_CURVE('',#4492,#4492,#3886,.T.);
#5394=EDGE_CURVE('',#4490,#4480,#2802,.T.);
#5395=EDGE_CURVE('',#4481,#4489,#2803,.T.);
#5396=EDGE_CURVE('',#4491,#4479,#2804,.T.);
#5397=EDGE_CURVE('',#4493,#4493,#3887,.T.);
#5398=EDGE_CURVE('',#4494,#4494,#3888,.T.);
#5399=EDGE_CURVE('',#4492,#4493,#2805,.T.);
#5400=EDGE_CURVE('',#4494,#4495,#2806,.T.);
#5401=EDGE_CURVE('',#4495,#4495,#3889,.T.);
#5402=EDGE_CURVE('',#4496,#4496,#3890,.T.);
#5403=EDGE_CURVE('',#4496,#4497,#2807,.T.);
#5404=EDGE_CURVE('',#4497,#4497,#3891,.T.);
#5405=EDGE_CURVE('',#4498,#4498,#3892,.T.);
#5406=EDGE_CURVE('',#4498,#4499,#2808,.T.);
#5407=EDGE_CURVE('',#4499,#4499,#3893,.T.);
#5408=EDGE_CURVE('',#4500,#4500,#3894,.T.);
#5409=EDGE_CURVE('',#4500,#4501,#2809,.T.);
#5410=EDGE_CURVE('',#4501,#4501,#3895,.T.);
#5411=EDGE_CURVE('',#4502,#4502,#3896,.T.);
#5412=EDGE_CURVE('',#4502,#4503,#2810,.T.);
#5413=EDGE_CURVE('',#4503,#4503,#3897,.T.);
#5414=EDGE_CURVE('',#4504,#4505,#2811,.T.);
#5415=EDGE_CURVE('',#4504,#4505,#3898,.T.);
#5416=EDGE_CURVE('',#4506,#4504,#491,.T.);
#5417=EDGE_CURVE('',#4507,#4506,#3899,.T.);
#5418=EDGE_CURVE('',#4508,#4507,#492,.T.);
#5419=EDGE_CURVE('',#4508,#4509,#2812,.T.);
#5420=EDGE_CURVE('',#4510,#4509,#493,.T.);
#5421=EDGE_CURVE('',#4509,#4510,#494,.T.);
#5422=EDGE_CURVE('',#4505,#4508,#495,.T.);
#5423=EDGE_CURVE('',#4507,#4506,#2813,.T.);
#5424=EDGE_CURVE('',#4511,#4511,#3900,.T.);
#5425=EDGE_CURVE('',#4511,#4512,#2814,.T.);
#5426=EDGE_CURVE('',#4512,#4512,#3901,.T.);
#5427=EDGE_CURVE('',#4513,#4513,#3902,.T.);
#5428=EDGE_CURVE('',#4513,#4514,#2815,.T.);
#5429=EDGE_CURVE('',#4514,#4514,#3903,.T.);
#5430=EDGE_CURVE('',#4515,#4515,#3904,.T.);
#5431=EDGE_CURVE('',#4515,#4516,#2816,.T.);
#5432=EDGE_CURVE('',#4516,#4516,#3905,.T.);
#5433=EDGE_CURVE('',#4517,#4517,#3906,.T.);
#5434=EDGE_CURVE('',#4518,#4518,#3907,.T.);
#5435=EDGE_CURVE('',#4519,#4519,#3908,.T.);
#5436=EDGE_CURVE('',#4520,#4520,#3909,.T.);
#5437=EDGE_CURVE('',#4517,#4519,#2817,.T.);
#5438=EDGE_CURVE('',#4520,#4521,#2818,.T.);
#5439=EDGE_CURVE('',#4521,#4521,#3910,.T.);
#5440=EDGE_CURVE('',#4522,#4522,#3911,.T.);
#5441=EDGE_CURVE('',#4522,#4518,#2819,.T.);
#5442=EDGE_CURVE('',#4523,#4523,#3912,.T.);
#5443=EDGE_CURVE('',#4523,#4524,#2820,.T.);
#5444=EDGE_CURVE('',#4524,#4524,#3913,.T.);
#5445=EDGE_CURVE('',#4525,#4525,#3914,.T.);
#5446=EDGE_CURVE('',#4525,#4526,#2821,.T.);
#5447=EDGE_CURVE('',#4526,#4526,#3915,.T.);
#5448=EDGE_CURVE('',#4527,#4527,#3916,.T.);
#5449=EDGE_CURVE('',#4527,#4528,#2822,.T.);
#5450=EDGE_CURVE('',#4528,#4528,#3917,.T.);
#5451=EDGE_CURVE('',#4529,#4529,#3918,.T.);
#5452=EDGE_CURVE('',#4529,#4530,#2823,.T.);
#5453=EDGE_CURVE('',#4530,#4530,#3919,.T.);
#5454=EDGE_CURVE('',#4531,#4531,#3920,.T.);
#5455=EDGE_CURVE('',#4531,#4532,#2824,.T.);
#5456=EDGE_CURVE('',#4532,#4532,#3921,.T.);
#5457=EDGE_CURVE('',#4533,#4533,#3922,.T.);
#5458=EDGE_CURVE('',#4533,#4534,#2825,.T.);
#5459=EDGE_CURVE('',#4534,#4534,#3923,.T.);
#5460=EDGE_CURVE('',#4535,#4535,#3924,.T.);
#5461=EDGE_CURVE('',#4535,#4536,#2826,.T.);
#5462=EDGE_CURVE('',#4536,#4536,#3925,.T.);
#5463=EDGE_CURVE('',#4537,#4537,#3926,.T.);
#5464=EDGE_CURVE('',#4538,#4538,#3927,.T.);
#5465=EDGE_CURVE('',#4539,#4539,#3928,.T.);
#5466=EDGE_CURVE('',#4540,#4540,#3929,.T.);
#5467=EDGE_CURVE('',#4537,#4539,#2827,.T.);
#5468=EDGE_CURVE('',#4540,#4541,#2828,.T.);
#5469=EDGE_CURVE('',#4541,#4541,#3930,.T.);
#5470=EDGE_CURVE('',#4542,#4542,#3931,.T.);
#5471=EDGE_CURVE('',#4542,#4538,#2829,.T.);
#5472=EDGE_CURVE('',#4543,#4543,#3932,.T.);
#5473=EDGE_CURVE('',#4543,#4544,#2830,.T.);
#5474=EDGE_CURVE('',#4544,#4544,#3933,.T.);
#5475=EDGE_CURVE('',#4545,#4545,#3934,.T.);
#5476=EDGE_CURVE('',#4545,#4546,#2831,.T.);
#5477=EDGE_CURVE('',#4546,#4546,#3935,.T.);
#5478=EDGE_CURVE('',#4547,#4547,#3936,.T.);
#5479=EDGE_CURVE('',#4547,#4548,#2832,.T.);
#5480=EDGE_CURVE('',#4548,#4548,#3937,.T.);
#5481=EDGE_CURVE('',#4549,#4549,#3938,.T.);
#5482=EDGE_CURVE('',#4549,#4550,#2833,.T.);
#5483=EDGE_CURVE('',#4550,#4550,#3939,.T.);
#5484=EDGE_CURVE('',#4551,#4551,#3940,.T.);
#5485=EDGE_CURVE('',#4551,#4552,#2834,.T.);
#5486=EDGE_CURVE('',#4552,#4552,#3941,.T.);
#5487=EDGE_CURVE('',#4553,#4553,#3942,.T.);
#5488=EDGE_CURVE('',#4553,#4554,#2835,.T.);
#5489=EDGE_CURVE('',#4554,#4554,#3943,.T.);
#5490=EDGE_CURVE('',#4555,#4555,#3944,.T.);
#5491=EDGE_CURVE('',#4556,#4556,#3945,.T.);
#5492=EDGE_CURVE('',#4556,#4555,#2836,.T.);
#5493=EDGE_CURVE('',#4557,#4557,#3946,.T.);
#5494=EDGE_CURVE('',#4557,#4556,#2837,.T.);
#5495=EDGE_CURVE('',#4558,#4558,#3947,.T.);
#5496=EDGE_CURVE('',#4558,#4557,#2838,.T.);
#5497=EDGE_CURVE('',#4559,#4559,#3948,.T.);
#5498=EDGE_CURVE('',#4560,#4560,#3949,.F.);
#5499=EDGE_CURVE('',#4560,#4559,#2839,.T.);
#5500=EDGE_CURVE('',#4561,#4561,#3950,.F.);
#5501=EDGE_CURVE('',#4561,#4560,#2840,.T.);
#5502=EDGE_CURVE('',#4562,#4562,#3951,.T.);
#5503=EDGE_CURVE('',#4562,#4561,#2841,.T.);
#5504=EDGE_CURVE('',#4563,#4564,#2842,.T.);
#5505=EDGE_CURVE('',#4564,#4565,#2843,.T.);
#5506=EDGE_CURVE('',#4565,#4566,#2844,.T.);
#5507=EDGE_CURVE('',#4563,#4566,#2845,.T.);
#5508=EDGE_CURVE('',#4564,#4567,#2846,.T.);
#5509=EDGE_CURVE('',#4567,#4568,#2847,.T.);
#5510=EDGE_CURVE('',#4568,#4565,#2848,.T.);
#5511=EDGE_CURVE('',#4567,#4569,#2849,.T.);
#5512=EDGE_CURVE('',#4569,#4570,#2850,.T.);
#5513=EDGE_CURVE('',#4570,#4568,#2851,.T.);
#5514=EDGE_CURVE('',#4569,#4571,#2852,.T.);
#5515=EDGE_CURVE('',#4571,#4572,#2853,.T.);
#5516=EDGE_CURVE('',#4572,#4570,#2854,.T.);
#5517=EDGE_CURVE('',#4571,#4573,#2855,.T.);
#5518=EDGE_CURVE('',#4573,#4574,#2856,.T.);
#5519=EDGE_CURVE('',#4574,#4572,#2857,.T.);
#5520=EDGE_CURVE('',#4573,#4563,#2858,.T.);
#5521=EDGE_CURVE('',#4566,#4574,#2859,.T.);
#5522=EDGE_CURVE('',#4575,#4575,#3952,.T.);
#5523=EDGE_CURVE('',#4576,#4577,#2860,.T.);
#5524=EDGE_CURVE('',#4576,#4578,#2861,.T.);
#5525=EDGE_CURVE('',#4578,#4579,#2862,.T.);
#5526=EDGE_CURVE('',#4577,#4579,#2863,.T.);
#5527=EDGE_CURVE('',#4580,#4576,#2864,.T.);
#5528=EDGE_CURVE('',#4580,#4581,#2865,.T.);
#5529=EDGE_CURVE('',#4581,#4578,#2866,.T.);
#5530=EDGE_CURVE('',#4582,#4580,#2867,.T.);
#5531=EDGE_CURVE('',#4582,#4583,#2868,.T.);
#5532=EDGE_CURVE('',#4583,#4581,#2869,.T.);
#5533=EDGE_CURVE('',#4584,#4582,#2870,.T.);
#5534=EDGE_CURVE('',#4584,#4585,#2871,.T.);
#5535=EDGE_CURVE('',#4585,#4583,#2872,.T.);
#5536=EDGE_CURVE('',#4586,#4584,#2873,.T.);
#5537=EDGE_CURVE('',#4586,#4587,#2874,.T.);
#5538=EDGE_CURVE('',#4587,#4585,#2875,.T.);
#5539=EDGE_CURVE('',#4577,#4586,#2876,.T.);
#5540=EDGE_CURVE('',#4579,#4587,#2877,.T.);
#5541=EDGE_CURVE('',#4588,#4588,#3953,.T.);
#5542=EDGE_CURVE('',#4589,#4589,#3954,.T.);
#5543=EDGE_CURVE('',#4589,#4588,#2878,.T.);
#5544=EDGE_CURVE('',#4575,#4589,#2879,.T.);
#5545=EDGE_CURVE('',#4590,#4590,#3955,.T.);
#5546=EDGE_CURVE('',#4590,#4591,#2880,.T.);
#5547=EDGE_CURVE('',#4591,#4591,#3956,.T.);
#5548=EDGE_CURVE('',#4592,#4592,#3957,.T.);
#5549=EDGE_CURVE('',#4592,#4593,#2881,.T.);
#5550=EDGE_CURVE('',#4593,#4593,#3958,.T.);
#5551=EDGE_CURVE('',#4594,#4595,#2882,.T.);
#5552=EDGE_CURVE('',#4596,#4594,#3959,.T.);
#5553=EDGE_CURVE('',#4597,#4596,#2883,.T.);
#5554=EDGE_CURVE('',#4597,#4595,#3960,.T.);
#5555=EDGE_CURVE('',#4598,#4595,#2884,.T.);
#5556=EDGE_CURVE('',#4599,#4598,#2885,.T.);
#5557=EDGE_CURVE('',#4594,#4599,#2886,.T.);
#5558=EDGE_CURVE('',#4597,#4600,#2887,.T.);
#5559=EDGE_CURVE('',#4598,#4600,#3961,.T.);
#5560=EDGE_CURVE('',#4601,#4596,#2888,.T.);
#5561=EDGE_CURVE('',#4600,#4601,#2889,.T.);
#5562=EDGE_CURVE('',#4599,#4601,#3962,.T.);
#5563=EDGE_CURVE('',#4602,#4602,#3963,.T.);
#5564=EDGE_CURVE('',#4602,#4603,#2890,.T.);
#5565=EDGE_CURVE('',#4603,#4603,#3964,.T.);
#5566=EDGE_CURVE('',#4604,#4604,#3965,.T.);
#5567=EDGE_CURVE('',#4604,#4605,#2891,.T.);
#5568=EDGE_CURVE('',#4605,#4605,#3966,.T.);
#5569=EDGE_CURVE('',#4606,#4606,#3967,.T.);
#5570=EDGE_CURVE('',#4606,#4607,#2892,.T.);
#5571=EDGE_CURVE('',#4607,#4607,#3968,.T.);
#5572=EDGE_CURVE('',#4608,#4608,#3969,.T.);
#5573=EDGE_CURVE('',#4608,#4609,#2893,.T.);
#5574=EDGE_CURVE('',#4609,#4609,#3970,.T.);
#5575=EDGE_CURVE('',#4610,#4610,#3971,.T.);
#5576=EDGE_CURVE('',#4610,#4611,#2894,.T.);
#5577=EDGE_CURVE('',#4611,#4611,#3972,.T.);
#5578=EDGE_CURVE('',#4612,#4612,#3973,.T.);
#5579=EDGE_CURVE('',#4612,#4613,#2895,.T.);
#5580=EDGE_CURVE('',#4613,#4613,#3974,.T.);
#5581=EDGE_CURVE('',#4614,#4615,#2896,.T.);
#5582=EDGE_CURVE('',#4616,#4614,#3975,.T.);
#5583=EDGE_CURVE('',#4617,#4616,#2897,.T.);
#5584=EDGE_CURVE('',#4617,#4615,#3976,.T.);
#5585=EDGE_CURVE('',#4618,#4615,#2898,.T.);
#5586=EDGE_CURVE('',#4619,#4618,#2899,.T.);
#5587=EDGE_CURVE('',#4614,#4619,#2900,.T.);
#5588=EDGE_CURVE('',#4617,#4620,#2901,.T.);
#5589=EDGE_CURVE('',#4618,#4620,#3977,.T.);
#5590=EDGE_CURVE('',#4621,#4616,#2902,.T.);
#5591=EDGE_CURVE('',#4620,#4621,#2903,.T.);
#5592=EDGE_CURVE('',#4619,#4621,#3978,.T.);
#5593=EDGE_CURVE('',#4622,#4622,#3979,.T.);
#5594=EDGE_CURVE('',#4622,#4623,#2904,.T.);
#5595=EDGE_CURVE('',#4623,#4623,#3980,.T.);
#5596=EDGE_CURVE('',#4624,#4624,#3981,.T.);
#5597=EDGE_CURVE('',#4624,#4625,#2905,.T.);
#5598=EDGE_CURVE('',#4625,#4625,#3982,.T.);
#5599=EDGE_CURVE('',#4626,#4626,#3983,.T.);
#5600=EDGE_CURVE('',#4626,#4627,#2906,.T.);
#5601=EDGE_CURVE('',#4627,#4627,#3984,.T.);
#5602=EDGE_CURVE('',#4628,#4628,#3985,.T.);
#5603=EDGE_CURVE('',#4628,#4629,#2907,.T.);
#5604=EDGE_CURVE('',#4629,#4629,#3986,.T.);
#5605=EDGE_CURVE('',#4630,#4630,#3987,.T.);
#5606=EDGE_CURVE('',#4630,#4631,#2908,.T.);
#5607=EDGE_CURVE('',#4631,#4631,#3988,.T.);
#5608=EDGE_CURVE('',#4632,#4632,#3989,.T.);
#5609=EDGE_CURVE('',#4632,#4633,#2909,.T.);
#5610=EDGE_CURVE('',#4633,#4633,#3990,.T.);
#5611=EDGE_CURVE('',#4634,#4634,#3991,.T.);
#5612=EDGE_CURVE('',#4634,#4635,#2910,.T.);
#5613=EDGE_CURVE('',#4635,#4635,#3992,.T.);
#5614=EDGE_CURVE('',#4636,#4636,#3993,.T.);
#5615=EDGE_CURVE('',#4636,#4637,#2911,.T.);
#5616=EDGE_CURVE('',#4637,#4637,#3994,.T.);
#5617=EDGE_CURVE('',#4638,#4638,#3995,.T.);
#5618=EDGE_CURVE('',#4638,#4639,#2912,.T.);
#5619=EDGE_CURVE('',#4639,#4639,#3996,.T.);
#5620=EDGE_CURVE('',#4640,#4640,#3997,.T.);
#5621=EDGE_CURVE('',#4640,#4641,#2913,.T.);
#5622=EDGE_CURVE('',#4641,#4641,#3998,.T.);
#5623=EDGE_CURVE('',#4642,#4643,#2914,.T.);
#5624=EDGE_CURVE('',#4643,#4644,#2915,.T.);
#5625=EDGE_CURVE('',#4645,#4644,#2916,.T.);
#5626=EDGE_CURVE('',#4642,#4645,#2917,.T.);
#5627=EDGE_CURVE('',#4646,#4642,#2918,.T.);
#5628=EDGE_CURVE('',#4647,#4645,#2919,.T.);
#5629=EDGE_CURVE('',#4646,#4647,#2920,.T.);
#5630=EDGE_CURVE('',#4648,#4646,#2921,.T.);
#5631=EDGE_CURVE('',#4649,#4647,#2922,.T.);
#5632=EDGE_CURVE('',#4648,#4649,#2923,.T.);
#5633=EDGE_CURVE('',#4643,#4648,#2924,.T.);
#5634=EDGE_CURVE('',#4644,#4649,#2925,.T.);
#5635=EDGE_CURVE('',#4650,#4650,#3999,.T.);
#5636=EDGE_CURVE('',#4650,#4651,#2926,.T.);
#5637=EDGE_CURVE('',#4651,#4651,#4000,.T.);
#5638=EDGE_CURVE('',#4652,#4652,#4001,.T.);
#5639=EDGE_CURVE('',#4652,#4653,#2927,.T.);
#5640=EDGE_CURVE('',#4653,#4653,#4002,.T.);
#5641=EDGE_CURVE('',#4654,#4654,#4003,.T.);
#5642=EDGE_CURVE('',#4654,#4655,#2928,.T.);
#5643=EDGE_CURVE('',#4655,#4655,#4004,.T.);
#5644=EDGE_CURVE('',#4656,#4656,#4005,.T.);
#5645=EDGE_CURVE('',#4656,#4657,#2929,.T.);
#5646=EDGE_CURVE('',#4657,#4657,#4006,.T.);
#5647=EDGE_CURVE('',#4658,#4658,#4007,.T.);
#5648=EDGE_CURVE('',#4658,#4659,#2930,.T.);
#5649=EDGE_CURVE('',#4659,#4659,#4008,.T.);
#5650=EDGE_CURVE('',#4660,#4661,#2931,.T.);
#5651=EDGE_CURVE('',#4661,#4662,#2932,.T.);
#5652=EDGE_CURVE('',#4663,#4662,#2933,.T.);
#5653=EDGE_CURVE('',#4660,#4663,#2934,.T.);
#5654=EDGE_CURVE('',#4664,#4660,#2935,.T.);
#5655=EDGE_CURVE('',#4665,#4663,#2936,.T.);
#5656=EDGE_CURVE('',#4664,#4665,#2937,.T.);
#5657=EDGE_CURVE('',#4666,#4664,#2938,.T.);
#5658=EDGE_CURVE('',#4667,#4665,#2939,.T.);
#5659=EDGE_CURVE('',#4666,#4667,#2940,.T.);
#5660=EDGE_CURVE('',#4661,#4666,#2941,.T.);
#5661=EDGE_CURVE('',#4662,#4667,#2942,.T.);
#5662=EDGE_CURVE('',#4668,#4668,#4009,.T.);
#5663=EDGE_CURVE('',#4668,#4669,#2943,.T.);
#5664=EDGE_CURVE('',#4669,#4669,#4010,.T.);
#5665=EDGE_CURVE('',#4670,#4670,#4011,.T.);
#5666=EDGE_CURVE('',#4670,#4671,#2944,.T.);
#5667=EDGE_CURVE('',#4671,#4671,#4012,.T.);
#5668=EDGE_CURVE('',#4672,#4672,#4013,.T.);
#5669=EDGE_CURVE('',#4672,#4673,#2945,.T.);
#5670=EDGE_CURVE('',#4673,#4673,#4014,.T.);
#5671=EDGE_CURVE('',#4674,#4674,#4015,.T.);
#5672=EDGE_CURVE('',#4674,#4675,#2946,.T.);
#5673=EDGE_CURVE('',#4675,#4675,#4016,.T.);
#5674=EDGE_CURVE('',#4676,#4676,#4017,.T.);
#5675=EDGE_CURVE('',#4676,#4677,#2947,.T.);
#5676=EDGE_CURVE('',#4677,#4677,#4018,.T.);
#5677=EDGE_CURVE('',#4678,#4679,#2948,.T.);
#5678=EDGE_CURVE('',#4679,#4680,#2949,.T.);
#5679=EDGE_CURVE('',#4681,#4680,#2950,.T.);
#5680=EDGE_CURVE('',#4678,#4681,#2951,.T.);
#5681=EDGE_CURVE('',#4682,#4678,#2952,.T.);
#5682=EDGE_CURVE('',#4683,#4681,#2953,.T.);
#5683=EDGE_CURVE('',#4682,#4683,#2954,.T.);
#5684=EDGE_CURVE('',#4684,#4682,#2955,.T.);
#5685=EDGE_CURVE('',#4685,#4683,#2956,.T.);
#5686=EDGE_CURVE('',#4684,#4685,#2957,.T.);
#5687=EDGE_CURVE('',#4679,#4684,#2958,.T.);
#5688=EDGE_CURVE('',#4680,#4685,#2959,.T.);
#5689=EDGE_CURVE('',#4686,#4686,#4019,.T.);
#5690=EDGE_CURVE('',#4686,#4687,#2960,.T.);
#5691=EDGE_CURVE('',#4687,#4687,#4020,.T.);
#5692=EDGE_CURVE('',#4688,#4688,#4021,.T.);
#5693=EDGE_CURVE('',#4689,#4689,#4022,.T.);
#5694=EDGE_CURVE('',#4690,#4690,#4023,.T.);
#5695=EDGE_CURVE('',#4691,#4691,#4024,.T.);
#5696=EDGE_CURVE('',#4688,#4690,#2961,.T.);
#5697=EDGE_CURVE('',#4691,#4692,#2962,.T.);
#5698=EDGE_CURVE('',#4692,#4692,#4025,.T.);
#5699=EDGE_CURVE('',#4693,#4693,#4026,.T.);
#5700=EDGE_CURVE('',#4693,#4689,#2963,.T.);
#5701=EDGE_CURVE('',#4694,#4694,#4027,.T.);
#5702=EDGE_CURVE('',#4694,#4695,#2964,.T.);
#5703=EDGE_CURVE('',#4695,#4695,#4028,.T.);
#5704=EDGE_CURVE('',#4696,#4696,#4029,.T.);
#5705=EDGE_CURVE('',#4696,#4697,#2965,.T.);
#5706=EDGE_CURVE('',#4697,#4697,#4030,.T.);
#5707=EDGE_CURVE('',#4698,#4698,#4031,.T.);
#5708=EDGE_CURVE('',#4698,#4699,#2966,.T.);
#5709=EDGE_CURVE('',#4699,#4699,#4032,.T.);
#5710=EDGE_CURVE('',#4700,#4700,#4033,.T.);
#5711=EDGE_CURVE('',#4700,#4701,#2967,.T.);
#5712=EDGE_CURVE('',#4701,#4701,#4034,.T.);
#5713=EDGE_CURVE('',#4702,#4702,#4035,.T.);
#5714=EDGE_CURVE('',#4702,#4703,#2968,.T.);
#5715=EDGE_CURVE('',#4703,#4703,#4036,.T.);
#5716=EDGE_CURVE('',#4704,#4704,#4037,.T.);
#5717=EDGE_CURVE('',#4704,#4705,#2969,.T.);
#5718=EDGE_CURVE('',#4705,#4705,#4038,.T.);
#5719=EDGE_CURVE('',#4706,#4706,#4039,.T.);
#5720=EDGE_CURVE('',#4706,#4707,#2970,.T.);
#5721=EDGE_CURVE('',#4707,#4707,#4040,.T.);
#5722=EDGE_CURVE('',#4708,#4708,#4041,.T.);
#5723=EDGE_CURVE('',#4708,#4709,#2971,.T.);
#5724=EDGE_CURVE('',#4709,#4709,#4042,.T.);
#5725=EDGE_CURVE('',#4710,#4710,#4043,.T.);
#5726=EDGE_CURVE('',#4710,#4711,#2972,.T.);
#5727=EDGE_CURVE('',#4711,#4711,#4044,.T.);
#5728=EDGE_CURVE('',#4712,#4712,#4045,.T.);
#5729=EDGE_CURVE('',#4712,#4713,#2973,.T.);
#5730=EDGE_CURVE('',#4713,#4713,#4046,.T.);
#5731=EDGE_CURVE('',#4714,#4714,#4047,.T.);
#5732=EDGE_CURVE('',#4714,#4715,#2974,.T.);
#5733=EDGE_CURVE('',#4715,#4715,#4048,.T.);
#5734=EDGE_CURVE('',#4716,#4716,#4049,.T.);
#5735=EDGE_CURVE('',#4716,#4717,#2975,.T.);
#5736=EDGE_CURVE('',#4717,#4717,#4050,.T.);
#5737=EDGE_CURVE('',#4718,#4719,#2976,.T.);
#5738=EDGE_CURVE('',#4719,#4720,#2977,.T.);
#5739=EDGE_CURVE('',#4721,#4720,#2978,.T.);
#5740=EDGE_CURVE('',#4718,#4721,#2979,.T.);
#5741=EDGE_CURVE('',#4722,#4718,#2980,.T.);
#5742=EDGE_CURVE('',#4723,#4721,#2981,.T.);
#5743=EDGE_CURVE('',#4722,#4723,#2982,.T.);
#5744=EDGE_CURVE('',#4724,#4722,#2983,.T.);
#5745=EDGE_CURVE('',#4725,#4723,#2984,.T.);
#5746=EDGE_CURVE('',#4724,#4725,#2985,.T.);
#5747=EDGE_CURVE('',#4719,#4724,#2986,.T.);
#5748=EDGE_CURVE('',#4720,#4725,#2987,.T.);
#5749=EDGE_CURVE('',#4726,#4726,#4051,.T.);
#5750=EDGE_CURVE('',#4726,#4727,#2988,.T.);
#5751=EDGE_CURVE('',#4727,#4727,#4052,.T.);
#5752=EDGE_CURVE('',#4728,#4728,#4053,.T.);
#5753=EDGE_CURVE('',#4728,#4729,#2989,.T.);
#5754=EDGE_CURVE('',#4729,#4729,#4054,.T.);
#5755=EDGE_CURVE('',#4730,#4730,#4055,.T.);
#5756=EDGE_CURVE('',#4730,#4731,#2990,.T.);
#5757=EDGE_CURVE('',#4731,#4731,#4056,.T.);
#5758=EDGE_CURVE('',#4732,#4732,#4057,.T.);
#5759=EDGE_CURVE('',#4732,#4733,#2991,.T.);
#5760=EDGE_CURVE('',#4733,#4733,#4058,.T.);
#5761=EDGE_CURVE('',#4734,#4734,#4059,.T.);
#5762=EDGE_CURVE('',#4734,#4735,#2992,.T.);
#5763=EDGE_CURVE('',#4735,#4735,#4060,.T.);
#5764=EDGE_CURVE('',#4736,#4737,#2993,.T.);
#5765=EDGE_CURVE('',#4737,#4738,#2994,.T.);
#5766=EDGE_CURVE('',#4739,#4738,#2995,.T.);
#5767=EDGE_CURVE('',#4736,#4739,#2996,.T.);
#5768=EDGE_CURVE('',#4740,#4736,#2997,.T.);
#5769=EDGE_CURVE('',#4741,#4739,#2998,.T.);
#5770=EDGE_CURVE('',#4740,#4741,#2999,.T.);
#5771=EDGE_CURVE('',#4742,#4740,#3000,.T.);
#5772=EDGE_CURVE('',#4743,#4741,#3001,.T.);
#5773=EDGE_CURVE('',#4742,#4743,#3002,.T.);
#5774=EDGE_CURVE('',#4737,#4742,#3003,.T.);
#5775=EDGE_CURVE('',#4738,#4743,#3004,.T.);
#5776=EDGE_CURVE('',#4744,#4744,#4061,.T.);
#5777=EDGE_CURVE('',#4744,#4745,#3005,.T.);
#5778=EDGE_CURVE('',#4745,#4745,#4062,.T.);
#5779=EDGE_CURVE('',#4746,#4746,#4063,.T.);
#5780=EDGE_CURVE('',#4746,#4747,#3006,.T.);
#5781=EDGE_CURVE('',#4747,#4747,#4064,.T.);
#5782=EDGE_CURVE('',#4748,#4748,#4065,.T.);
#5783=EDGE_CURVE('',#4748,#4749,#3007,.T.);
#5784=EDGE_CURVE('',#4749,#4749,#4066,.T.);
#5785=EDGE_CURVE('',#4750,#4750,#4067,.T.);
#5786=EDGE_CURVE('',#4750,#4751,#3008,.T.);
#5787=EDGE_CURVE('',#4751,#4751,#4068,.T.);
#5788=EDGE_CURVE('',#4752,#4752,#4069,.T.);
#5789=EDGE_CURVE('',#4752,#4753,#3009,.T.);
#5790=EDGE_CURVE('',#4753,#4753,#4070,.T.);
#5791=EDGE_CURVE('',#4754,#4755,#3010,.T.);
#5792=EDGE_CURVE('',#4755,#4756,#3011,.T.);
#5793=EDGE_CURVE('',#4757,#4756,#3012,.T.);
#5794=EDGE_CURVE('',#4754,#4757,#3013,.T.);
#5795=EDGE_CURVE('',#4758,#4754,#3014,.T.);
#5796=EDGE_CURVE('',#4759,#4757,#3015,.T.);
#5797=EDGE_CURVE('',#4758,#4759,#3016,.T.);
#5798=EDGE_CURVE('',#4760,#4758,#3017,.T.);
#5799=EDGE_CURVE('',#4761,#4759,#3018,.T.);
#5800=EDGE_CURVE('',#4760,#4761,#3019,.T.);
#5801=EDGE_CURVE('',#4755,#4760,#3020,.T.);
#5802=EDGE_CURVE('',#4756,#4761,#3021,.T.);
#5803=EDGE_CURVE('',#4762,#4762,#4071,.T.);
#5804=EDGE_CURVE('',#4762,#4763,#3022,.T.);
#5805=EDGE_CURVE('',#4763,#4763,#4072,.T.);
#5806=EDGE_CURVE('',#4764,#4764,#4073,.T.);
#5807=EDGE_CURVE('',#4765,#4765,#4074,.T.);
#5808=EDGE_CURVE('',#4766,#4766,#4075,.T.);
#5809=EDGE_CURVE('',#4767,#4767,#4076,.T.);
#5810=EDGE_CURVE('',#4764,#4766,#3023,.T.);
#5811=EDGE_CURVE('',#4767,#4768,#3024,.T.);
#5812=EDGE_CURVE('',#4768,#4768,#4077,.T.);
#5813=EDGE_CURVE('',#4769,#4769,#4078,.T.);
#5814=EDGE_CURVE('',#4769,#4765,#3025,.T.);
#5815=EDGE_CURVE('',#4770,#4770,#4079,.T.);
#5816=EDGE_CURVE('',#4770,#4771,#3026,.T.);
#5817=EDGE_CURVE('',#4771,#4771,#4080,.T.);
#5818=EDGE_CURVE('',#4772,#4772,#4081,.T.);
#5819=EDGE_CURVE('',#4772,#4773,#3027,.T.);
#5820=EDGE_CURVE('',#4773,#4773,#4082,.T.);
#5821=EDGE_CURVE('',#4774,#4774,#4083,.T.);
#5822=EDGE_CURVE('',#4774,#4775,#3028,.T.);
#5823=EDGE_CURVE('',#4775,#4775,#4084,.T.);
#5824=EDGE_CURVE('',#4776,#4776,#4085,.T.);
#5825=EDGE_CURVE('',#4776,#4777,#3029,.T.);
#5826=EDGE_CURVE('',#4777,#4777,#4086,.T.);
#5827=EDGE_CURVE('',#4778,#4778,#4087,.T.);
#5828=EDGE_CURVE('',#4778,#4779,#3030,.T.);
#5829=EDGE_CURVE('',#4779,#4779,#4088,.T.);
#5830=EDGE_CURVE('',#4780,#4780,#4089,.T.);
#5831=EDGE_CURVE('',#4780,#4781,#3031,.T.);
#5832=EDGE_CURVE('',#4781,#4781,#4090,.T.);
#5833=EDGE_CURVE('',#4782,#4783,#4091,.T.);
#5834=EDGE_CURVE('',#4784,#4782,#3032,.T.);
#5835=EDGE_CURVE('',#4785,#4784,#3033,.T.);
#5836=EDGE_CURVE('',#4783,#4785,#3034,.T.);
#5837=EDGE_CURVE('',#4783,#4786,#3035,.T.);
#5838=EDGE_CURVE('',#4787,#4785,#3036,.T.);
#5839=EDGE_CURVE('',#4787,#4786,#3037,.T.);
#5840=EDGE_CURVE('',#4786,#4788,#4092,.T.);
#5841=EDGE_CURVE('',#4789,#4787,#3038,.T.);
#5842=EDGE_CURVE('',#4788,#4789,#3039,.T.);
#5843=EDGE_CURVE('',#4788,#4782,#3040,.T.);
#5844=EDGE_CURVE('',#4789,#4784,#3041,.T.);
#5845=EDGE_CURVE('',#4790,#4790,#4093,.T.);
#5846=EDGE_CURVE('',#4791,#4791,#4094,.T.);
#5847=EDGE_CURVE('',#4792,#4792,#4095,.T.);
#5848=EDGE_CURVE('',#4792,#4790,#3042,.T.);
#5849=EDGE_CURVE('',#4793,#4793,#4096,.T.);
#5850=EDGE_CURVE('',#4794,#4794,#4097,.T.);
#5851=EDGE_CURVE('',#4794,#4793,#3043,.T.);
#5852=EDGE_CURVE('',#4795,#4795,#4098,.T.);
#5853=EDGE_CURVE('',#4796,#4796,#4099,.T.);
#5854=EDGE_CURVE('',#4796,#4795,#3044,.T.);
#5855=EDGE_CURVE('',#4797,#4797,#4100,.T.);
#5856=EDGE_CURVE('',#4798,#4798,#4101,.T.);
#5857=EDGE_CURVE('',#4798,#4797,#3045,.T.);
#5858=EDGE_CURVE('',#4799,#4799,#4102,.T.);
#5859=EDGE_CURVE('',#4800,#4800,#4103,.T.);
#5860=EDGE_CURVE('',#4800,#4799,#3046,.T.);
#5861=EDGE_CURVE('',#4801,#4801,#4104,.T.);
#5862=EDGE_CURVE('',#4801,#4791,#3047,.T.);
#5863=EDGE_CURVE('',#4802,#4803,#4105,.T.);
#5864=EDGE_CURVE('',#4804,#4802,#3048,.T.);
#5865=EDGE_CURVE('',#4805,#4804,#4106,.T.);
#5866=EDGE_CURVE('',#4803,#4805,#3049,.T.);
#5867=EDGE_CURVE('',#4803,#4806,#3050,.T.);
#5868=EDGE_CURVE('',#4807,#4805,#3051,.T.);
#5869=EDGE_CURVE('',#4807,#4806,#3052,.T.);
#5870=EDGE_CURVE('',#4806,#4808,#4107,.T.);
#5871=EDGE_CURVE('',#4809,#4807,#4108,.T.);
#5872=EDGE_CURVE('',#4808,#4809,#3053,.T.);
#5873=EDGE_CURVE('',#4808,#4802,#3054,.T.);
#5874=EDGE_CURVE('',#4804,#4809,#3055,.T.);
#5875=EDGE_CURVE('',#4810,#4810,#4109,.T.);
#5876=EDGE_CURVE('',#4811,#4811,#4110,.T.);
#5877=EDGE_CURVE('',#4812,#4812,#4111,.T.);
#5878=EDGE_CURVE('',#4812,#4810,#3056,.T.);
#5879=EDGE_CURVE('',#4813,#4813,#4112,.T.);
#5880=EDGE_CURVE('',#4813,#4811,#3057,.T.);
#5881=EDGE_CURVE('',#4814,#4815,#3058,.T.);
#5882=EDGE_CURVE('',#4815,#4816,#3059,.T.);
#5883=EDGE_CURVE('',#4816,#4817,#3060,.T.);
#5884=EDGE_CURVE('',#4814,#4817,#3061,.T.);
#5885=EDGE_CURVE('',#4815,#4818,#3062,.T.);
#5886=EDGE_CURVE('',#4818,#4819,#3063,.T.);
#5887=EDGE_CURVE('',#4819,#4816,#3064,.T.);
#5888=EDGE_CURVE('',#4818,#4820,#3065,.T.);
#5889=EDGE_CURVE('',#4820,#4821,#3066,.T.);
#5890=EDGE_CURVE('',#4821,#4819,#3067,.T.);
#5891=EDGE_CURVE('',#4820,#4822,#3068,.T.);
#5892=EDGE_CURVE('',#4822,#4823,#3069,.T.);
#5893=EDGE_CURVE('',#4823,#4821,#3070,.T.);
#5894=EDGE_CURVE('',#4822,#4824,#3071,.T.);
#5895=EDGE_CURVE('',#4824,#4825,#3072,.T.);
#5896=EDGE_CURVE('',#4825,#4823,#3073,.T.);
#5897=EDGE_CURVE('',#4824,#4814,#3074,.T.);
#5898=EDGE_CURVE('',#4817,#4825,#3075,.T.);
#5899=EDGE_CURVE('',#4826,#4826,#4113,.T.);
#5900=EDGE_CURVE('',#4827,#4827,#4114,.T.);
#5901=EDGE_CURVE('',#4828,#4828,#4115,.T.);
#5902=EDGE_CURVE('',#4828,#4827,#3076,.T.);
#5903=EDGE_CURVE('',#4829,#4829,#4116,.T.);
#5904=EDGE_CURVE('',#4829,#4828,#3077,.T.);
#5905=EDGE_CURVE('',#4830,#4830,#4117,.T.);
#5906=EDGE_CURVE('',#4830,#4829,#3078,.T.);
#5907=EDGE_CURVE('',#4831,#4831,#4118,.T.);
#5908=EDGE_CURVE('',#4832,#4832,#4119,.F.);
#5909=EDGE_CURVE('',#4832,#4831,#3079,.T.);
#5910=EDGE_CURVE('',#4826,#4832,#3080,.T.);
#5911=ORIENTED_EDGE('',*,*,#4833,.F.);
#5912=ORIENTED_EDGE('',*,*,#4834,.T.);
#5913=ORIENTED_EDGE('',*,*,#4835,.F.);
#5914=ORIENTED_EDGE('',*,*,#4834,.F.);
#5915=ORIENTED_EDGE('',*,*,#4836,.F.);
#5916=ORIENTED_EDGE('',*,*,#4837,.T.);
#5917=ORIENTED_EDGE('',*,*,#4838,.F.);
#5918=ORIENTED_EDGE('',*,*,#4837,.F.);
#5919=ORIENTED_EDGE('',*,*,#4839,.F.);
#5920=ORIENTED_EDGE('',*,*,#4840,.T.);
#5921=ORIENTED_EDGE('',*,*,#4841,.F.);
#5922=ORIENTED_EDGE('',*,*,#4840,.F.);
#5923=ORIENTED_EDGE('',*,*,#4842,.F.);
#5924=ORIENTED_EDGE('',*,*,#4843,.T.);
#5925=ORIENTED_EDGE('',*,*,#4844,.F.);
#5926=ORIENTED_EDGE('',*,*,#4843,.F.);
#5927=ORIENTED_EDGE('',*,*,#4845,.F.);
#5928=ORIENTED_EDGE('',*,*,#4846,.T.);
#5929=ORIENTED_EDGE('',*,*,#4847,.F.);
#5930=ORIENTED_EDGE('',*,*,#4846,.F.);
#5931=ORIENTED_EDGE('',*,*,#4848,.F.);
#5932=ORIENTED_EDGE('',*,*,#4849,.T.);
#5933=ORIENTED_EDGE('',*,*,#4850,.F.);
#5934=ORIENTED_EDGE('',*,*,#4849,.F.);
#5935=ORIENTED_EDGE('',*,*,#4851,.F.);
#5936=ORIENTED_EDGE('',*,*,#4852,.T.);
#5937=ORIENTED_EDGE('',*,*,#4853,.F.);
#5938=ORIENTED_EDGE('',*,*,#4852,.F.);
#5939=ORIENTED_EDGE('',*,*,#4854,.F.);
#5940=ORIENTED_EDGE('',*,*,#4855,.T.);
#5941=ORIENTED_EDGE('',*,*,#4856,.F.);
#5942=ORIENTED_EDGE('',*,*,#4855,.F.);
#5943=ORIENTED_EDGE('',*,*,#4857,.F.);
#5944=ORIENTED_EDGE('',*,*,#4858,.T.);
#5945=ORIENTED_EDGE('',*,*,#4859,.F.);
#5946=ORIENTED_EDGE('',*,*,#4858,.F.);
#5947=ORIENTED_EDGE('',*,*,#4860,.F.);
#5948=ORIENTED_EDGE('',*,*,#4861,.T.);
#5949=ORIENTED_EDGE('',*,*,#4862,.F.);
#5950=ORIENTED_EDGE('',*,*,#4861,.F.);
#5951=ORIENTED_EDGE('',*,*,#4863,.F.);
#5952=ORIENTED_EDGE('',*,*,#4864,.T.);
#5953=ORIENTED_EDGE('',*,*,#4865,.F.);
#5954=ORIENTED_EDGE('',*,*,#4864,.F.);
#5955=ORIENTED_EDGE('',*,*,#4866,.F.);
#5956=ORIENTED_EDGE('',*,*,#4867,.T.);
#5957=ORIENTED_EDGE('',*,*,#4868,.F.);
#5958=ORIENTED_EDGE('',*,*,#4867,.F.);
#5959=ORIENTED_EDGE('',*,*,#4869,.T.);
#5960=ORIENTED_EDGE('',*,*,#4870,.T.);
#5961=ORIENTED_EDGE('',*,*,#4871,.F.);
#5962=ORIENTED_EDGE('',*,*,#4872,.F.);
#5963=ORIENTED_EDGE('',*,*,#4873,.T.);
#5964=ORIENTED_EDGE('',*,*,#4872,.T.);
#5965=ORIENTED_EDGE('',*,*,#4874,.F.);
#5966=ORIENTED_EDGE('',*,*,#4875,.F.);
#5967=ORIENTED_EDGE('',*,*,#4876,.T.);
#5968=ORIENTED_EDGE('',*,*,#4875,.T.);
#5969=ORIENTED_EDGE('',*,*,#4877,.F.);
#5970=ORIENTED_EDGE('',*,*,#4878,.F.);
#5971=ORIENTED_EDGE('',*,*,#4879,.T.);
#5972=ORIENTED_EDGE('',*,*,#4878,.T.);
#5973=ORIENTED_EDGE('',*,*,#4880,.F.);
#5974=ORIENTED_EDGE('',*,*,#4870,.F.);
#5975=ORIENTED_EDGE('',*,*,#4880,.T.);
#5976=ORIENTED_EDGE('',*,*,#4877,.T.);
#5977=ORIENTED_EDGE('',*,*,#4874,.T.);
#5978=ORIENTED_EDGE('',*,*,#4871,.T.);
#5979=ORIENTED_EDGE('',*,*,#4841,.T.);
#5980=ORIENTED_EDGE('',*,*,#4844,.T.);
#5981=ORIENTED_EDGE('',*,*,#4868,.T.);
#5982=ORIENTED_EDGE('',*,*,#4865,.T.);
#5983=ORIENTED_EDGE('',*,*,#4862,.T.);
#5984=ORIENTED_EDGE('',*,*,#4859,.T.);
#5985=ORIENTED_EDGE('',*,*,#4856,.T.);
#5986=ORIENTED_EDGE('',*,*,#4853,.T.);
#5987=ORIENTED_EDGE('',*,*,#4850,.T.);
#5988=ORIENTED_EDGE('',*,*,#4847,.T.);
#5989=ORIENTED_EDGE('',*,*,#4838,.T.);
#5990=ORIENTED_EDGE('',*,*,#4835,.T.);
#5991=ORIENTED_EDGE('',*,*,#4879,.F.);
#5992=ORIENTED_EDGE('',*,*,#4869,.F.);
#5993=ORIENTED_EDGE('',*,*,#4873,.F.);
#5994=ORIENTED_EDGE('',*,*,#4876,.F.);
#5995=ORIENTED_EDGE('',*,*,#4839,.T.);
#5996=ORIENTED_EDGE('',*,*,#4842,.T.);
#5997=ORIENTED_EDGE('',*,*,#4866,.T.);
#5998=ORIENTED_EDGE('',*,*,#4863,.T.);
#5999=ORIENTED_EDGE('',*,*,#4860,.T.);
#6000=ORIENTED_EDGE('',*,*,#4857,.T.);
#6001=ORIENTED_EDGE('',*,*,#4854,.T.);
#6002=ORIENTED_EDGE('',*,*,#4851,.T.);
#6003=ORIENTED_EDGE('',*,*,#4848,.T.);
#6004=ORIENTED_EDGE('',*,*,#4845,.T.);
#6005=ORIENTED_EDGE('',*,*,#4836,.T.);
#6006=ORIENTED_EDGE('',*,*,#4833,.T.);
#6007=ORIENTED_EDGE('',*,*,#4881,.T.);
#6008=ORIENTED_EDGE('',*,*,#4882,.T.);
#6009=ORIENTED_EDGE('',*,*,#4883,.F.);
#6010=ORIENTED_EDGE('',*,*,#4884,.F.);
#6011=ORIENTED_EDGE('',*,*,#4885,.T.);
#6012=ORIENTED_EDGE('',*,*,#4884,.T.);
#6013=ORIENTED_EDGE('',*,*,#4886,.F.);
#6014=ORIENTED_EDGE('',*,*,#4887,.F.);
#6015=ORIENTED_EDGE('',*,*,#4888,.T.);
#6016=ORIENTED_EDGE('',*,*,#4887,.T.);
#6017=ORIENTED_EDGE('',*,*,#4889,.F.);
#6018=ORIENTED_EDGE('',*,*,#4890,.F.);
#6019=ORIENTED_EDGE('',*,*,#4891,.T.);
#6020=ORIENTED_EDGE('',*,*,#4890,.T.);
#6021=ORIENTED_EDGE('',*,*,#4892,.F.);
#6022=ORIENTED_EDGE('',*,*,#4882,.F.);
#6023=ORIENTED_EDGE('',*,*,#4892,.T.);
#6024=ORIENTED_EDGE('',*,*,#4889,.T.);
#6025=ORIENTED_EDGE('',*,*,#4886,.T.);
#6026=ORIENTED_EDGE('',*,*,#4883,.T.);
#6027=ORIENTED_EDGE('',*,*,#4891,.F.);
#6028=ORIENTED_EDGE('',*,*,#4881,.F.);
#6029=ORIENTED_EDGE('',*,*,#4885,.F.);
#6030=ORIENTED_EDGE('',*,*,#4888,.F.);
#6031=ORIENTED_EDGE('',*,*,#4893,.T.);
#6032=ORIENTED_EDGE('',*,*,#4894,.T.);
#6033=ORIENTED_EDGE('',*,*,#4895,.F.);
#6034=ORIENTED_EDGE('',*,*,#4896,.F.);
#6035=ORIENTED_EDGE('',*,*,#4897,.T.);
#6036=ORIENTED_EDGE('',*,*,#4896,.T.);
#6037=ORIENTED_EDGE('',*,*,#4898,.F.);
#6038=ORIENTED_EDGE('',*,*,#4899,.F.);
#6039=ORIENTED_EDGE('',*,*,#4900,.T.);
#6040=ORIENTED_EDGE('',*,*,#4899,.T.);
#6041=ORIENTED_EDGE('',*,*,#4901,.F.);
#6042=ORIENTED_EDGE('',*,*,#4902,.F.);
#6043=ORIENTED_EDGE('',*,*,#4903,.T.);
#6044=ORIENTED_EDGE('',*,*,#4902,.T.);
#6045=ORIENTED_EDGE('',*,*,#4904,.F.);
#6046=ORIENTED_EDGE('',*,*,#4894,.F.);
#6047=ORIENTED_EDGE('',*,*,#4904,.T.);
#6048=ORIENTED_EDGE('',*,*,#4901,.T.);
#6049=ORIENTED_EDGE('',*,*,#4898,.T.);
#6050=ORIENTED_EDGE('',*,*,#4895,.T.);
#6051=ORIENTED_EDGE('',*,*,#4903,.F.);
#6052=ORIENTED_EDGE('',*,*,#4893,.F.);
#6053=ORIENTED_EDGE('',*,*,#4897,.F.);
#6054=ORIENTED_EDGE('',*,*,#4900,.F.);
#6055=ORIENTED_EDGE('',*,*,#4905,.F.);
#6056=ORIENTED_EDGE('',*,*,#4906,.F.);
#6057=ORIENTED_EDGE('',*,*,#4907,.T.);
#6058=ORIENTED_EDGE('',*,*,#4908,.F.);
#6059=ORIENTED_EDGE('',*,*,#4909,.F.);
#6060=ORIENTED_EDGE('',*,*,#4907,.F.);
#6061=ORIENTED_EDGE('',*,*,#4910,.F.);
#6062=ORIENTED_EDGE('',*,*,#4911,.T.);
#6063=ORIENTED_EDGE('',*,*,#4912,.F.);
#6064=ORIENTED_EDGE('',*,*,#4911,.F.);
#6065=ORIENTED_EDGE('',*,*,#4910,.T.);
#6066=ORIENTED_EDGE('',*,*,#4913,.F.);
#6067=ORIENTED_EDGE('',*,*,#4914,.T.);
#6068=ORIENTED_EDGE('',*,*,#4915,.F.);
#6069=ORIENTED_EDGE('',*,*,#4914,.F.);
#6070=ORIENTED_EDGE('',*,*,#4913,.T.);
#6071=ORIENTED_EDGE('',*,*,#4916,.F.);
#6072=ORIENTED_EDGE('',*,*,#4917,.T.);
#6073=ORIENTED_EDGE('',*,*,#4918,.F.);
#6074=ORIENTED_EDGE('',*,*,#4917,.F.);
#6075=ORIENTED_EDGE('',*,*,#4916,.T.);
#6076=ORIENTED_EDGE('',*,*,#4919,.F.);
#6077=ORIENTED_EDGE('',*,*,#4920,.T.);
#6078=ORIENTED_EDGE('',*,*,#4921,.F.);
#6079=ORIENTED_EDGE('',*,*,#4920,.F.);
#6080=ORIENTED_EDGE('',*,*,#4919,.T.);
#6081=ORIENTED_EDGE('',*,*,#4922,.F.);
#6082=ORIENTED_EDGE('',*,*,#4923,.F.);
#6083=ORIENTED_EDGE('',*,*,#4924,.F.);
#6084=ORIENTED_EDGE('',*,*,#4925,.F.);
#6085=ORIENTED_EDGE('',*,*,#4926,.F.);
#6086=ORIENTED_EDGE('',*,*,#4923,.T.);
#6087=ORIENTED_EDGE('',*,*,#4927,.F.);
#6088=ORIENTED_EDGE('',*,*,#4928,.T.);
#6089=ORIENTED_EDGE('',*,*,#4929,.F.);
#6090=ORIENTED_EDGE('',*,*,#4930,.F.);
#6091=ORIENTED_EDGE('',*,*,#4931,.F.);
#6092=ORIENTED_EDGE('',*,*,#4928,.F.);
#6093=ORIENTED_EDGE('',*,*,#4932,.F.);
#6094=ORIENTED_EDGE('',*,*,#4933,.T.);
#6095=ORIENTED_EDGE('',*,*,#4934,.F.);
#6096=ORIENTED_EDGE('',*,*,#4935,.F.);
#6097=ORIENTED_EDGE('',*,*,#4936,.F.);
#6098=ORIENTED_EDGE('',*,*,#4933,.F.);
#6099=ORIENTED_EDGE('',*,*,#4937,.F.);
#6100=ORIENTED_EDGE('',*,*,#4938,.T.);
#6101=ORIENTED_EDGE('',*,*,#4939,.F.);
#6102=ORIENTED_EDGE('',*,*,#4940,.F.);
#6103=ORIENTED_EDGE('',*,*,#4941,.F.);
#6104=ORIENTED_EDGE('',*,*,#4938,.F.);
#6105=ORIENTED_EDGE('',*,*,#4942,.F.);
#6106=ORIENTED_EDGE('',*,*,#4943,.T.);
#6107=ORIENTED_EDGE('',*,*,#4944,.T.);
#6108=ORIENTED_EDGE('',*,*,#4924,.T.);
#6109=ORIENTED_EDGE('',*,*,#4922,.T.);
#6110=ORIENTED_EDGE('',*,*,#4926,.T.);
#6111=ORIENTED_EDGE('',*,*,#4945,.T.);
#6112=ORIENTED_EDGE('',*,*,#4939,.T.);
#6113=ORIENTED_EDGE('',*,*,#4941,.T.);
#6114=ORIENTED_EDGE('',*,*,#4937,.T.);
#6115=ORIENTED_EDGE('',*,*,#4946,.T.);
#6116=ORIENTED_EDGE('',*,*,#4934,.T.);
#6117=ORIENTED_EDGE('',*,*,#4936,.T.);
#6118=ORIENTED_EDGE('',*,*,#4932,.T.);
#6119=ORIENTED_EDGE('',*,*,#4947,.T.);
#6120=ORIENTED_EDGE('',*,*,#4929,.T.);
#6121=ORIENTED_EDGE('',*,*,#4931,.T.);
#6122=ORIENTED_EDGE('',*,*,#4927,.T.);
#6123=ORIENTED_EDGE('',*,*,#4948,.T.);
#6124=ORIENTED_EDGE('',*,*,#4943,.F.);
#6125=ORIENTED_EDGE('',*,*,#4949,.T.);
#6126=ORIENTED_EDGE('',*,*,#4948,.F.);
#6127=ORIENTED_EDGE('',*,*,#4930,.T.);
#6128=ORIENTED_EDGE('',*,*,#4947,.F.);
#6129=ORIENTED_EDGE('',*,*,#4935,.T.);
#6130=ORIENTED_EDGE('',*,*,#4946,.F.);
#6131=ORIENTED_EDGE('',*,*,#4940,.T.);
#6132=ORIENTED_EDGE('',*,*,#4945,.F.);
#6133=ORIENTED_EDGE('',*,*,#4925,.T.);
#6134=ORIENTED_EDGE('',*,*,#4944,.F.);
#6135=ORIENTED_EDGE('',*,*,#4950,.T.);
#6136=ORIENTED_EDGE('',*,*,#4951,.T.);
#6137=ORIENTED_EDGE('',*,*,#4952,.T.);
#6138=ORIENTED_EDGE('',*,*,#4953,.T.);
#6139=ORIENTED_EDGE('',*,*,#4954,.F.);
#6140=ORIENTED_EDGE('',*,*,#4955,.T.);
#6141=ORIENTED_EDGE('',*,*,#4950,.F.);
#6142=ORIENTED_EDGE('',*,*,#4955,.F.);
#6143=ORIENTED_EDGE('',*,*,#4956,.F.);
#6144=ORIENTED_EDGE('',*,*,#4957,.T.);
#6145=ORIENTED_EDGE('',*,*,#4953,.F.);
#6146=ORIENTED_EDGE('',*,*,#4957,.F.);
#6147=ORIENTED_EDGE('',*,*,#4958,.F.);
#6148=ORIENTED_EDGE('',*,*,#4959,.T.);
#6149=ORIENTED_EDGE('',*,*,#4951,.F.);
#6150=ORIENTED_EDGE('',*,*,#4959,.F.);
#6151=ORIENTED_EDGE('',*,*,#4960,.F.);
#6152=ORIENTED_EDGE('',*,*,#4961,.T.);
#6153=ORIENTED_EDGE('',*,*,#4952,.F.);
#6154=ORIENTED_EDGE('',*,*,#4961,.F.);
#6155=ORIENTED_EDGE('',*,*,#4962,.F.);
#6156=ORIENTED_EDGE('',*,*,#4963,.T.);
#6157=ORIENTED_EDGE('',*,*,#4964,.F.);
#6158=ORIENTED_EDGE('',*,*,#4963,.F.);
#6159=ORIENTED_EDGE('',*,*,#4962,.T.);
#6160=ORIENTED_EDGE('',*,*,#4965,.F.);
#6161=ORIENTED_EDGE('',*,*,#4949,.F.);
#6162=ORIENTED_EDGE('',*,*,#4966,.T.);
#6163=ORIENTED_EDGE('',*,*,#4967,.T.);
#6164=ORIENTED_EDGE('',*,*,#4966,.F.);
#6165=ORIENTED_EDGE('',*,*,#4908,.T.);
#6166=ORIENTED_EDGE('',*,*,#4909,.T.);
#6167=ORIENTED_EDGE('',*,*,#4965,.T.);
#6168=ORIENTED_EDGE('',*,*,#4968,.T.);
#6169=ORIENTED_EDGE('',*,*,#4969,.T.);
#6170=ORIENTED_EDGE('',*,*,#4968,.F.);
#6171=ORIENTED_EDGE('',*,*,#4905,.T.);
#6172=ORIENTED_EDGE('',*,*,#4906,.T.);
#6173=ORIENTED_EDGE('',*,*,#4942,.T.);
#6174=ORIENTED_EDGE('',*,*,#4964,.T.);
#6175=ORIENTED_EDGE('',*,*,#4921,.T.);
#6176=ORIENTED_EDGE('',*,*,#4918,.T.);
#6177=ORIENTED_EDGE('',*,*,#4915,.T.);
#6178=ORIENTED_EDGE('',*,*,#4912,.T.);
#6179=ORIENTED_EDGE('',*,*,#4967,.F.);
#6180=ORIENTED_EDGE('',*,*,#4969,.F.);
#6181=ORIENTED_EDGE('',*,*,#4960,.T.);
#6182=ORIENTED_EDGE('',*,*,#4958,.T.);
#6183=ORIENTED_EDGE('',*,*,#4956,.T.);
#6184=ORIENTED_EDGE('',*,*,#4954,.T.);
#6185=ORIENTED_EDGE('',*,*,#4970,.F.);
#6186=ORIENTED_EDGE('',*,*,#4971,.T.);
#6187=ORIENTED_EDGE('',*,*,#4972,.F.);
#6188=ORIENTED_EDGE('',*,*,#4971,.F.);
#6189=ORIENTED_EDGE('',*,*,#4970,.T.);
#6190=ORIENTED_EDGE('',*,*,#4973,.F.);
#6191=ORIENTED_EDGE('',*,*,#4974,.F.);
#6192=ORIENTED_EDGE('',*,*,#4975,.T.);
#6193=ORIENTED_EDGE('',*,*,#4976,.F.);
#6194=ORIENTED_EDGE('',*,*,#4975,.F.);
#6195=ORIENTED_EDGE('',*,*,#4974,.T.);
#6196=ORIENTED_EDGE('',*,*,#4977,.F.);
#6197=ORIENTED_EDGE('',*,*,#4978,.F.);
#6198=ORIENTED_EDGE('',*,*,#4979,.T.);
#6199=ORIENTED_EDGE('',*,*,#4980,.F.);
#6200=ORIENTED_EDGE('',*,*,#4979,.F.);
#6201=ORIENTED_EDGE('',*,*,#4978,.T.);
#6202=ORIENTED_EDGE('',*,*,#4981,.F.);
#6203=ORIENTED_EDGE('',*,*,#4982,.F.);
#6204=ORIENTED_EDGE('',*,*,#4983,.T.);
#6205=ORIENTED_EDGE('',*,*,#4984,.F.);
#6206=ORIENTED_EDGE('',*,*,#4983,.F.);
#6207=ORIENTED_EDGE('',*,*,#4982,.T.);
#6208=ORIENTED_EDGE('',*,*,#4985,.F.);
#6209=ORIENTED_EDGE('',*,*,#4986,.F.);
#6210=ORIENTED_EDGE('',*,*,#4987,.T.);
#6211=ORIENTED_EDGE('',*,*,#4973,.T.);
#6212=ORIENTED_EDGE('',*,*,#4987,.F.);
#6213=ORIENTED_EDGE('',*,*,#4988,.F.);
#6214=ORIENTED_EDGE('',*,*,#4989,.T.);
#6215=ORIENTED_EDGE('',*,*,#4977,.T.);
#6216=ORIENTED_EDGE('',*,*,#4989,.F.);
#6217=ORIENTED_EDGE('',*,*,#4990,.F.);
#6218=ORIENTED_EDGE('',*,*,#4991,.T.);
#6219=ORIENTED_EDGE('',*,*,#4981,.T.);
#6220=ORIENTED_EDGE('',*,*,#4991,.F.);
#6221=ORIENTED_EDGE('',*,*,#4992,.F.);
#6222=ORIENTED_EDGE('',*,*,#4993,.T.);
#6223=ORIENTED_EDGE('',*,*,#4985,.T.);
#6224=ORIENTED_EDGE('',*,*,#4993,.F.);
#6225=ORIENTED_EDGE('',*,*,#4994,.F.);
#6226=ORIENTED_EDGE('',*,*,#4995,.T.);
#6227=ORIENTED_EDGE('',*,*,#4996,.T.);
#6228=ORIENTED_EDGE('',*,*,#4995,.F.);
#6229=ORIENTED_EDGE('',*,*,#4996,.F.);
#6230=ORIENTED_EDGE('',*,*,#4997,.F.);
#6231=ORIENTED_EDGE('',*,*,#4998,.F.);
#6232=ORIENTED_EDGE('',*,*,#4999,.T.);
#6233=ORIENTED_EDGE('',*,*,#4997,.T.);
#6234=ORIENTED_EDGE('',*,*,#4999,.F.);
#6235=ORIENTED_EDGE('',*,*,#5000,.F.);
#6236=ORIENTED_EDGE('',*,*,#5001,.T.);
#6237=ORIENTED_EDGE('',*,*,#5002,.T.);
#6238=ORIENTED_EDGE('',*,*,#5001,.F.);
#6239=ORIENTED_EDGE('',*,*,#5000,.T.);
#6240=ORIENTED_EDGE('',*,*,#4998,.T.);
#6241=ORIENTED_EDGE('',*,*,#4984,.T.);
#6242=ORIENTED_EDGE('',*,*,#4980,.T.);
#6243=ORIENTED_EDGE('',*,*,#4976,.T.);
#6244=ORIENTED_EDGE('',*,*,#4972,.T.);
#6245=ORIENTED_EDGE('',*,*,#5002,.F.);
#6246=ORIENTED_EDGE('',*,*,#4994,.T.);
#6247=ORIENTED_EDGE('',*,*,#4992,.T.);
#6248=ORIENTED_EDGE('',*,*,#4990,.T.);
#6249=ORIENTED_EDGE('',*,*,#4988,.T.);
#6250=ORIENTED_EDGE('',*,*,#4986,.T.);
#6251=ORIENTED_EDGE('',*,*,#5003,.F.);
#6252=ORIENTED_EDGE('',*,*,#5004,.F.);
#6253=ORIENTED_EDGE('',*,*,#5005,.T.);
#6254=ORIENTED_EDGE('',*,*,#5006,.F.);
#6255=ORIENTED_EDGE('',*,*,#5007,.F.);
#6256=ORIENTED_EDGE('',*,*,#5008,.F.);
#6257=ORIENTED_EDGE('',*,*,#5009,.T.);
#6258=ORIENTED_EDGE('',*,*,#5010,.F.);
#6259=ORIENTED_EDGE('',*,*,#5011,.F.);
#6260=ORIENTED_EDGE('',*,*,#5012,.T.);
#6261=ORIENTED_EDGE('',*,*,#5013,.F.);
#6262=ORIENTED_EDGE('',*,*,#5014,.F.);
#6263=ORIENTED_EDGE('',*,*,#5015,.F.);
#6264=ORIENTED_EDGE('',*,*,#5016,.F.);
#6265=ORIENTED_EDGE('',*,*,#5012,.F.);
#6266=ORIENTED_EDGE('',*,*,#5017,.F.);
#6267=ORIENTED_EDGE('',*,*,#5018,.T.);
#6268=ORIENTED_EDGE('',*,*,#5019,.F.);
#6269=ORIENTED_EDGE('',*,*,#5018,.F.);
#6270=ORIENTED_EDGE('',*,*,#5020,.F.);
#6271=ORIENTED_EDGE('',*,*,#5014,.T.);
#6272=ORIENTED_EDGE('',*,*,#5007,.T.);
#6273=ORIENTED_EDGE('',*,*,#5021,.F.);
#6274=ORIENTED_EDGE('',*,*,#5022,.F.);
#6275=ORIENTED_EDGE('',*,*,#5023,.F.);
#6276=ORIENTED_EDGE('',*,*,#5008,.T.);
#6277=ORIENTED_EDGE('',*,*,#5023,.T.);
#6278=ORIENTED_EDGE('',*,*,#5024,.F.);
#6279=ORIENTED_EDGE('',*,*,#5003,.T.);
#6280=ORIENTED_EDGE('',*,*,#5025,.F.);
#6281=ORIENTED_EDGE('',*,*,#5026,.F.);
#6282=ORIENTED_EDGE('',*,*,#5027,.F.);
#6283=ORIENTED_EDGE('',*,*,#5004,.T.);
#6284=ORIENTED_EDGE('',*,*,#5027,.T.);
#6285=ORIENTED_EDGE('',*,*,#5028,.F.);
#6286=ORIENTED_EDGE('',*,*,#5029,.T.);
#6287=ORIENTED_EDGE('',*,*,#5030,.T.);
#6288=ORIENTED_EDGE('',*,*,#5021,.T.);
#6289=ORIENTED_EDGE('',*,*,#5010,.T.);
#6290=ORIENTED_EDGE('',*,*,#5031,.T.);
#6291=ORIENTED_EDGE('',*,*,#5032,.T.);
#6292=ORIENTED_EDGE('',*,*,#5033,.T.);
#6293=ORIENTED_EDGE('',*,*,#5025,.T.);
#6294=ORIENTED_EDGE('',*,*,#5006,.T.);
#6295=ORIENTED_EDGE('',*,*,#5034,.T.);
#6296=ORIENTED_EDGE('',*,*,#5019,.T.);
#6297=ORIENTED_EDGE('',*,*,#5035,.F.);
#6298=ORIENTED_EDGE('',*,*,#5036,.T.);
#6299=ORIENTED_EDGE('',*,*,#5024,.T.);
#6300=ORIENTED_EDGE('',*,*,#5036,.F.);
#6301=ORIENTED_EDGE('',*,*,#5037,.F.);
#6302=ORIENTED_EDGE('',*,*,#5038,.T.);
#6303=ORIENTED_EDGE('',*,*,#5028,.T.);
#6304=ORIENTED_EDGE('',*,*,#5038,.F.);
#6305=ORIENTED_EDGE('',*,*,#5039,.F.);
#6306=ORIENTED_EDGE('',*,*,#5040,.T.);
#6307=ORIENTED_EDGE('',*,*,#5017,.T.);
#6308=ORIENTED_EDGE('',*,*,#5011,.T.);
#6309=ORIENTED_EDGE('',*,*,#5016,.T.);
#6310=ORIENTED_EDGE('',*,*,#5041,.T.);
#6311=ORIENTED_EDGE('',*,*,#5042,.F.);
#6312=ORIENTED_EDGE('',*,*,#5041,.F.);
#6313=ORIENTED_EDGE('',*,*,#5015,.T.);
#6314=ORIENTED_EDGE('',*,*,#5020,.T.);
#6315=ORIENTED_EDGE('',*,*,#5013,.T.);
#6316=ORIENTED_EDGE('',*,*,#5040,.F.);
#6317=ORIENTED_EDGE('',*,*,#5043,.T.);
#6318=ORIENTED_EDGE('',*,*,#5044,.T.);
#6319=ORIENTED_EDGE('',*,*,#5034,.F.);
#6320=ORIENTED_EDGE('',*,*,#5005,.F.);
#6321=ORIENTED_EDGE('',*,*,#5026,.T.);
#6322=ORIENTED_EDGE('',*,*,#5033,.F.);
#6323=ORIENTED_EDGE('',*,*,#5045,.F.);
#6324=ORIENTED_EDGE('',*,*,#5046,.T.);
#6325=ORIENTED_EDGE('',*,*,#5045,.T.);
#6326=ORIENTED_EDGE('',*,*,#5032,.F.);
#6327=ORIENTED_EDGE('',*,*,#5047,.F.);
#6328=ORIENTED_EDGE('',*,*,#5042,.T.);
#6329=ORIENTED_EDGE('',*,*,#5048,.T.);
#6330=ORIENTED_EDGE('',*,*,#5047,.T.);
#6331=ORIENTED_EDGE('',*,*,#5031,.F.);
#6332=ORIENTED_EDGE('',*,*,#5009,.F.);
#6333=ORIENTED_EDGE('',*,*,#5022,.T.);
#6334=ORIENTED_EDGE('',*,*,#5030,.F.);
#6335=ORIENTED_EDGE('',*,*,#5049,.F.);
#6336=ORIENTED_EDGE('',*,*,#5050,.T.);
#6337=ORIENTED_EDGE('',*,*,#5049,.T.);
#6338=ORIENTED_EDGE('',*,*,#5029,.F.);
#6339=ORIENTED_EDGE('',*,*,#5044,.F.);
#6340=ORIENTED_EDGE('',*,*,#5039,.T.);
#6341=ORIENTED_EDGE('',*,*,#5050,.F.);
#6342=ORIENTED_EDGE('',*,*,#5043,.F.);
#6343=ORIENTED_EDGE('',*,*,#5046,.F.);
#6344=ORIENTED_EDGE('',*,*,#5048,.F.);
#6345=ORIENTED_EDGE('',*,*,#5035,.T.);
#6346=ORIENTED_EDGE('',*,*,#5037,.T.);
#6347=ORIENTED_EDGE('',*,*,#5051,.F.);
#6348=ORIENTED_EDGE('',*,*,#5052,.F.);
#6349=ORIENTED_EDGE('',*,*,#5053,.T.);
#6350=ORIENTED_EDGE('',*,*,#5054,.F.);
#6351=ORIENTED_EDGE('',*,*,#5055,.F.);
#6352=ORIENTED_EDGE('',*,*,#5056,.F.);
#6353=ORIENTED_EDGE('',*,*,#5057,.T.);
#6354=ORIENTED_EDGE('',*,*,#5058,.F.);
#6355=ORIENTED_EDGE('',*,*,#5059,.F.);
#6356=ORIENTED_EDGE('',*,*,#5060,.T.);
#6357=ORIENTED_EDGE('',*,*,#5061,.F.);
#6358=ORIENTED_EDGE('',*,*,#5062,.F.);
#6359=ORIENTED_EDGE('',*,*,#5063,.F.);
#6360=ORIENTED_EDGE('',*,*,#5064,.F.);
#6361=ORIENTED_EDGE('',*,*,#5060,.F.);
#6362=ORIENTED_EDGE('',*,*,#5065,.F.);
#6363=ORIENTED_EDGE('',*,*,#5066,.T.);
#6364=ORIENTED_EDGE('',*,*,#5067,.F.);
#6365=ORIENTED_EDGE('',*,*,#5066,.F.);
#6366=ORIENTED_EDGE('',*,*,#5068,.F.);
#6367=ORIENTED_EDGE('',*,*,#5062,.T.);
#6368=ORIENTED_EDGE('',*,*,#5055,.T.);
#6369=ORIENTED_EDGE('',*,*,#5069,.F.);
#6370=ORIENTED_EDGE('',*,*,#5070,.F.);
#6371=ORIENTED_EDGE('',*,*,#5071,.F.);
#6372=ORIENTED_EDGE('',*,*,#5056,.T.);
#6373=ORIENTED_EDGE('',*,*,#5071,.T.);
#6374=ORIENTED_EDGE('',*,*,#5072,.F.);
#6375=ORIENTED_EDGE('',*,*,#5051,.T.);
#6376=ORIENTED_EDGE('',*,*,#5073,.F.);
#6377=ORIENTED_EDGE('',*,*,#5074,.F.);
#6378=ORIENTED_EDGE('',*,*,#5075,.F.);
#6379=ORIENTED_EDGE('',*,*,#5052,.T.);
#6380=ORIENTED_EDGE('',*,*,#5075,.T.);
#6381=ORIENTED_EDGE('',*,*,#5076,.F.);
#6382=ORIENTED_EDGE('',*,*,#5077,.T.);
#6383=ORIENTED_EDGE('',*,*,#5078,.T.);
#6384=ORIENTED_EDGE('',*,*,#5069,.T.);
#6385=ORIENTED_EDGE('',*,*,#5058,.T.);
#6386=ORIENTED_EDGE('',*,*,#5079,.T.);
#6387=ORIENTED_EDGE('',*,*,#5080,.T.);
#6388=ORIENTED_EDGE('',*,*,#5081,.T.);
#6389=ORIENTED_EDGE('',*,*,#5073,.T.);
#6390=ORIENTED_EDGE('',*,*,#5054,.T.);
#6391=ORIENTED_EDGE('',*,*,#5082,.T.);
#6392=ORIENTED_EDGE('',*,*,#5067,.T.);
#6393=ORIENTED_EDGE('',*,*,#5083,.F.);
#6394=ORIENTED_EDGE('',*,*,#5084,.T.);
#6395=ORIENTED_EDGE('',*,*,#5072,.T.);
#6396=ORIENTED_EDGE('',*,*,#5084,.F.);
#6397=ORIENTED_EDGE('',*,*,#5085,.F.);
#6398=ORIENTED_EDGE('',*,*,#5086,.T.);
#6399=ORIENTED_EDGE('',*,*,#5076,.T.);
#6400=ORIENTED_EDGE('',*,*,#5086,.F.);
#6401=ORIENTED_EDGE('',*,*,#5087,.F.);
#6402=ORIENTED_EDGE('',*,*,#5088,.T.);
#6403=ORIENTED_EDGE('',*,*,#5065,.T.);
#6404=ORIENTED_EDGE('',*,*,#5059,.T.);
#6405=ORIENTED_EDGE('',*,*,#5064,.T.);
#6406=ORIENTED_EDGE('',*,*,#5089,.T.);
#6407=ORIENTED_EDGE('',*,*,#5090,.F.);
#6408=ORIENTED_EDGE('',*,*,#5089,.F.);
#6409=ORIENTED_EDGE('',*,*,#5063,.T.);
#6410=ORIENTED_EDGE('',*,*,#5068,.T.);
#6411=ORIENTED_EDGE('',*,*,#5061,.T.);
#6412=ORIENTED_EDGE('',*,*,#5088,.F.);
#6413=ORIENTED_EDGE('',*,*,#5091,.T.);
#6414=ORIENTED_EDGE('',*,*,#5092,.T.);
#6415=ORIENTED_EDGE('',*,*,#5082,.F.);
#6416=ORIENTED_EDGE('',*,*,#5053,.F.);
#6417=ORIENTED_EDGE('',*,*,#5074,.T.);
#6418=ORIENTED_EDGE('',*,*,#5081,.F.);
#6419=ORIENTED_EDGE('',*,*,#5093,.F.);
#6420=ORIENTED_EDGE('',*,*,#5094,.T.);
#6421=ORIENTED_EDGE('',*,*,#5093,.T.);
#6422=ORIENTED_EDGE('',*,*,#5080,.F.);
#6423=ORIENTED_EDGE('',*,*,#5095,.F.);
#6424=ORIENTED_EDGE('',*,*,#5090,.T.);
#6425=ORIENTED_EDGE('',*,*,#5096,.T.);
#6426=ORIENTED_EDGE('',*,*,#5095,.T.);
#6427=ORIENTED_EDGE('',*,*,#5079,.F.);
#6428=ORIENTED_EDGE('',*,*,#5057,.F.);
#6429=ORIENTED_EDGE('',*,*,#5070,.T.);
#6430=ORIENTED_EDGE('',*,*,#5078,.F.);
#6431=ORIENTED_EDGE('',*,*,#5097,.F.);
#6432=ORIENTED_EDGE('',*,*,#5098,.T.);
#6433=ORIENTED_EDGE('',*,*,#5097,.T.);
#6434=ORIENTED_EDGE('',*,*,#5077,.F.);
#6435=ORIENTED_EDGE('',*,*,#5092,.F.);
#6436=ORIENTED_EDGE('',*,*,#5087,.T.);
#6437=ORIENTED_EDGE('',*,*,#5098,.F.);
#6438=ORIENTED_EDGE('',*,*,#5091,.F.);
#6439=ORIENTED_EDGE('',*,*,#5094,.F.);
#6440=ORIENTED_EDGE('',*,*,#5096,.F.);
#6441=ORIENTED_EDGE('',*,*,#5083,.T.);
#6442=ORIENTED_EDGE('',*,*,#5085,.T.);
#6443=ORIENTED_EDGE('',*,*,#5099,.F.);
#6444=ORIENTED_EDGE('',*,*,#5100,.F.);
#6445=ORIENTED_EDGE('',*,*,#5101,.T.);
#6446=ORIENTED_EDGE('',*,*,#5102,.F.);
#6447=ORIENTED_EDGE('',*,*,#5103,.F.);
#6448=ORIENTED_EDGE('',*,*,#5104,.T.);
#6449=ORIENTED_EDGE('',*,*,#5105,.F.);
#6450=ORIENTED_EDGE('',*,*,#5106,.F.);
#6451=ORIENTED_EDGE('',*,*,#5107,.T.);
#6452=ORIENTED_EDGE('',*,*,#5108,.F.);
#6453=ORIENTED_EDGE('',*,*,#5107,.F.);
#6454=ORIENTED_EDGE('',*,*,#5109,.F.);
#6455=ORIENTED_EDGE('',*,*,#5110,.F.);
#6456=ORIENTED_EDGE('',*,*,#5104,.F.);
#6457=ORIENTED_EDGE('',*,*,#5111,.F.);
#6458=ORIENTED_EDGE('',*,*,#5109,.T.);
#6459=ORIENTED_EDGE('',*,*,#5106,.T.);
#6460=ORIENTED_EDGE('',*,*,#5112,.F.);
#6461=ORIENTED_EDGE('',*,*,#5113,.T.);
#6462=ORIENTED_EDGE('',*,*,#5114,.F.);
#6463=ORIENTED_EDGE('',*,*,#5115,.F.);
#6464=ORIENTED_EDGE('',*,*,#5112,.T.);
#6465=ORIENTED_EDGE('',*,*,#5116,.F.);
#6466=ORIENTED_EDGE('',*,*,#5099,.T.);
#6467=ORIENTED_EDGE('',*,*,#5117,.F.);
#6468=ORIENTED_EDGE('',*,*,#5118,.F.);
#6469=ORIENTED_EDGE('',*,*,#5119,.F.);
#6470=ORIENTED_EDGE('',*,*,#5100,.T.);
#6471=ORIENTED_EDGE('',*,*,#5119,.T.);
#6472=ORIENTED_EDGE('',*,*,#5120,.F.);
#6473=ORIENTED_EDGE('',*,*,#5121,.T.);
#6474=ORIENTED_EDGE('',*,*,#5114,.T.);
#6475=ORIENTED_EDGE('',*,*,#5122,.T.);
#6476=ORIENTED_EDGE('',*,*,#5123,.T.);
#6477=ORIENTED_EDGE('',*,*,#5124,.T.);
#6478=ORIENTED_EDGE('',*,*,#5117,.T.);
#6479=ORIENTED_EDGE('',*,*,#5102,.T.);
#6480=ORIENTED_EDGE('',*,*,#5125,.T.);
#6481=ORIENTED_EDGE('',*,*,#5126,.T.);
#6482=ORIENTED_EDGE('',*,*,#5108,.T.);
#6483=ORIENTED_EDGE('',*,*,#5127,.F.);
#6484=ORIENTED_EDGE('',*,*,#5128,.T.);
#6485=ORIENTED_EDGE('',*,*,#5116,.T.);
#6486=ORIENTED_EDGE('',*,*,#5128,.F.);
#6487=ORIENTED_EDGE('',*,*,#5129,.F.);
#6488=ORIENTED_EDGE('',*,*,#5130,.T.);
#6489=ORIENTED_EDGE('',*,*,#5120,.T.);
#6490=ORIENTED_EDGE('',*,*,#5130,.F.);
#6491=ORIENTED_EDGE('',*,*,#5131,.F.);
#6492=ORIENTED_EDGE('',*,*,#5132,.T.);
#6493=ORIENTED_EDGE('',*,*,#5133,.F.);
#6494=ORIENTED_EDGE('',*,*,#5132,.F.);
#6495=ORIENTED_EDGE('',*,*,#5110,.T.);
#6496=ORIENTED_EDGE('',*,*,#5111,.T.);
#6497=ORIENTED_EDGE('',*,*,#5105,.T.);
#6498=ORIENTED_EDGE('',*,*,#5103,.T.);
#6499=ORIENTED_EDGE('',*,*,#5134,.T.);
#6500=ORIENTED_EDGE('',*,*,#5135,.T.);
#6501=ORIENTED_EDGE('',*,*,#5126,.F.);
#6502=ORIENTED_EDGE('',*,*,#5136,.F.);
#6503=ORIENTED_EDGE('',*,*,#5133,.T.);
#6504=ORIENTED_EDGE('',*,*,#5137,.T.);
#6505=ORIENTED_EDGE('',*,*,#5136,.T.);
#6506=ORIENTED_EDGE('',*,*,#5125,.F.);
#6507=ORIENTED_EDGE('',*,*,#5101,.F.);
#6508=ORIENTED_EDGE('',*,*,#5118,.T.);
#6509=ORIENTED_EDGE('',*,*,#5124,.F.);
#6510=ORIENTED_EDGE('',*,*,#5138,.F.);
#6511=ORIENTED_EDGE('',*,*,#5139,.T.);
#6512=ORIENTED_EDGE('',*,*,#5138,.T.);
#6513=ORIENTED_EDGE('',*,*,#5123,.F.);
#6514=ORIENTED_EDGE('',*,*,#5140,.F.);
#6515=ORIENTED_EDGE('',*,*,#5131,.T.);
#6516=ORIENTED_EDGE('',*,*,#5141,.T.);
#6517=ORIENTED_EDGE('',*,*,#5140,.T.);
#6518=ORIENTED_EDGE('',*,*,#5122,.F.);
#6519=ORIENTED_EDGE('',*,*,#5113,.F.);
#6520=ORIENTED_EDGE('',*,*,#5115,.T.);
#6521=ORIENTED_EDGE('',*,*,#5121,.F.);
#6522=ORIENTED_EDGE('',*,*,#5135,.F.);
#6523=ORIENTED_EDGE('',*,*,#5141,.F.);
#6524=ORIENTED_EDGE('',*,*,#5134,.F.);
#6525=ORIENTED_EDGE('',*,*,#5137,.F.);
#6526=ORIENTED_EDGE('',*,*,#5139,.F.);
#6527=ORIENTED_EDGE('',*,*,#5127,.T.);
#6528=ORIENTED_EDGE('',*,*,#5129,.T.);
#6529=ORIENTED_EDGE('',*,*,#5142,.F.);
#6530=ORIENTED_EDGE('',*,*,#5143,.F.);
#6531=ORIENTED_EDGE('',*,*,#5144,.T.);
#6532=ORIENTED_EDGE('',*,*,#5145,.F.);
#6533=ORIENTED_EDGE('',*,*,#5146,.F.);
#6534=ORIENTED_EDGE('',*,*,#5147,.T.);
#6535=ORIENTED_EDGE('',*,*,#5148,.F.);
#6536=ORIENTED_EDGE('',*,*,#5149,.F.);
#6537=ORIENTED_EDGE('',*,*,#5150,.T.);
#6538=ORIENTED_EDGE('',*,*,#5151,.F.);
#6539=ORIENTED_EDGE('',*,*,#5150,.F.);
#6540=ORIENTED_EDGE('',*,*,#5152,.F.);
#6541=ORIENTED_EDGE('',*,*,#5153,.F.);
#6542=ORIENTED_EDGE('',*,*,#5147,.F.);
#6543=ORIENTED_EDGE('',*,*,#5154,.F.);
#6544=ORIENTED_EDGE('',*,*,#5152,.T.);
#6545=ORIENTED_EDGE('',*,*,#5149,.T.);
#6546=ORIENTED_EDGE('',*,*,#5155,.F.);
#6547=ORIENTED_EDGE('',*,*,#5156,.T.);
#6548=ORIENTED_EDGE('',*,*,#5157,.F.);
#6549=ORIENTED_EDGE('',*,*,#5158,.F.);
#6550=ORIENTED_EDGE('',*,*,#5155,.T.);
#6551=ORIENTED_EDGE('',*,*,#5159,.F.);
#6552=ORIENTED_EDGE('',*,*,#5142,.T.);
#6553=ORIENTED_EDGE('',*,*,#5160,.F.);
#6554=ORIENTED_EDGE('',*,*,#5161,.F.);
#6555=ORIENTED_EDGE('',*,*,#5162,.F.);
#6556=ORIENTED_EDGE('',*,*,#5143,.T.);
#6557=ORIENTED_EDGE('',*,*,#5162,.T.);
#6558=ORIENTED_EDGE('',*,*,#5163,.F.);
#6559=ORIENTED_EDGE('',*,*,#5164,.T.);
#6560=ORIENTED_EDGE('',*,*,#5157,.T.);
#6561=ORIENTED_EDGE('',*,*,#5165,.T.);
#6562=ORIENTED_EDGE('',*,*,#5166,.T.);
#6563=ORIENTED_EDGE('',*,*,#5167,.T.);
#6564=ORIENTED_EDGE('',*,*,#5160,.T.);
#6565=ORIENTED_EDGE('',*,*,#5145,.T.);
#6566=ORIENTED_EDGE('',*,*,#5168,.T.);
#6567=ORIENTED_EDGE('',*,*,#5169,.T.);
#6568=ORIENTED_EDGE('',*,*,#5151,.T.);
#6569=ORIENTED_EDGE('',*,*,#5170,.F.);
#6570=ORIENTED_EDGE('',*,*,#5171,.T.);
#6571=ORIENTED_EDGE('',*,*,#5159,.T.);
#6572=ORIENTED_EDGE('',*,*,#5171,.F.);
#6573=ORIENTED_EDGE('',*,*,#5172,.F.);
#6574=ORIENTED_EDGE('',*,*,#5173,.T.);
#6575=ORIENTED_EDGE('',*,*,#5163,.T.);
#6576=ORIENTED_EDGE('',*,*,#5173,.F.);
#6577=ORIENTED_EDGE('',*,*,#5174,.F.);
#6578=ORIENTED_EDGE('',*,*,#5175,.T.);
#6579=ORIENTED_EDGE('',*,*,#5176,.F.);
#6580=ORIENTED_EDGE('',*,*,#5175,.F.);
#6581=ORIENTED_EDGE('',*,*,#5153,.T.);
#6582=ORIENTED_EDGE('',*,*,#5154,.T.);
#6583=ORIENTED_EDGE('',*,*,#5148,.T.);
#6584=ORIENTED_EDGE('',*,*,#5146,.T.);
#6585=ORIENTED_EDGE('',*,*,#5177,.T.);
#6586=ORIENTED_EDGE('',*,*,#5178,.T.);
#6587=ORIENTED_EDGE('',*,*,#5169,.F.);
#6588=ORIENTED_EDGE('',*,*,#5179,.F.);
#6589=ORIENTED_EDGE('',*,*,#5176,.T.);
#6590=ORIENTED_EDGE('',*,*,#5180,.T.);
#6591=ORIENTED_EDGE('',*,*,#5179,.T.);
#6592=ORIENTED_EDGE('',*,*,#5168,.F.);
#6593=ORIENTED_EDGE('',*,*,#5144,.F.);
#6594=ORIENTED_EDGE('',*,*,#5161,.T.);
#6595=ORIENTED_EDGE('',*,*,#5167,.F.);
#6596=ORIENTED_EDGE('',*,*,#5181,.F.);
#6597=ORIENTED_EDGE('',*,*,#5182,.T.);
#6598=ORIENTED_EDGE('',*,*,#5181,.T.);
#6599=ORIENTED_EDGE('',*,*,#5166,.F.);
#6600=ORIENTED_EDGE('',*,*,#5183,.F.);
#6601=ORIENTED_EDGE('',*,*,#5174,.T.);
#6602=ORIENTED_EDGE('',*,*,#5184,.T.);
#6603=ORIENTED_EDGE('',*,*,#5183,.T.);
#6604=ORIENTED_EDGE('',*,*,#5165,.F.);
#6605=ORIENTED_EDGE('',*,*,#5156,.F.);
#6606=ORIENTED_EDGE('',*,*,#5158,.T.);
#6607=ORIENTED_EDGE('',*,*,#5164,.F.);
#6608=ORIENTED_EDGE('',*,*,#5178,.F.);
#6609=ORIENTED_EDGE('',*,*,#5184,.F.);
#6610=ORIENTED_EDGE('',*,*,#5177,.F.);
#6611=ORIENTED_EDGE('',*,*,#5180,.F.);
#6612=ORIENTED_EDGE('',*,*,#5182,.F.);
#6613=ORIENTED_EDGE('',*,*,#5170,.T.);
#6614=ORIENTED_EDGE('',*,*,#5172,.T.);
#6615=ORIENTED_EDGE('',*,*,#5185,.T.);
#6616=ORIENTED_EDGE('',*,*,#5186,.T.);
#6617=ORIENTED_EDGE('',*,*,#5187,.T.);
#6618=ORIENTED_EDGE('',*,*,#5188,.F.);
#6619=ORIENTED_EDGE('',*,*,#5189,.T.);
#6620=ORIENTED_EDGE('',*,*,#5190,.T.);
#6621=ORIENTED_EDGE('',*,*,#5191,.T.);
#6622=ORIENTED_EDGE('',*,*,#5186,.F.);
#6623=ORIENTED_EDGE('',*,*,#5192,.T.);
#6624=ORIENTED_EDGE('',*,*,#5193,.T.);
#6625=ORIENTED_EDGE('',*,*,#5194,.T.);
#6626=ORIENTED_EDGE('',*,*,#5190,.F.);
#6627=ORIENTED_EDGE('',*,*,#5195,.T.);
#6628=ORIENTED_EDGE('',*,*,#5196,.T.);
#6629=ORIENTED_EDGE('',*,*,#5197,.T.);
#6630=ORIENTED_EDGE('',*,*,#5193,.F.);
#6631=ORIENTED_EDGE('',*,*,#5198,.T.);
#6632=ORIENTED_EDGE('',*,*,#5199,.T.);
#6633=ORIENTED_EDGE('',*,*,#5200,.T.);
#6634=ORIENTED_EDGE('',*,*,#5196,.F.);
#6635=ORIENTED_EDGE('',*,*,#5201,.T.);
#6636=ORIENTED_EDGE('',*,*,#5188,.T.);
#6637=ORIENTED_EDGE('',*,*,#5202,.T.);
#6638=ORIENTED_EDGE('',*,*,#5199,.F.);
#6639=ORIENTED_EDGE('',*,*,#5201,.F.);
#6640=ORIENTED_EDGE('',*,*,#5198,.F.);
#6641=ORIENTED_EDGE('',*,*,#5195,.F.);
#6642=ORIENTED_EDGE('',*,*,#5192,.F.);
#6643=ORIENTED_EDGE('',*,*,#5189,.F.);
#6644=ORIENTED_EDGE('',*,*,#5185,.F.);
#6645=ORIENTED_EDGE('',*,*,#5202,.F.);
#6646=ORIENTED_EDGE('',*,*,#5187,.F.);
#6647=ORIENTED_EDGE('',*,*,#5191,.F.);
#6648=ORIENTED_EDGE('',*,*,#5194,.F.);
#6649=ORIENTED_EDGE('',*,*,#5197,.F.);
#6650=ORIENTED_EDGE('',*,*,#5200,.F.);
#6651=ORIENTED_EDGE('',*,*,#5203,.F.);
#6652=ORIENTED_EDGE('',*,*,#5204,.F.);
#6653=ORIENTED_EDGE('',*,*,#5205,.F.);
#6654=ORIENTED_EDGE('',*,*,#5206,.T.);
#6655=ORIENTED_EDGE('',*,*,#5204,.T.);
#6656=ORIENTED_EDGE('',*,*,#5206,.F.);
#6657=ORIENTED_EDGE('',*,*,#5207,.F.);
#6658=ORIENTED_EDGE('',*,*,#5208,.T.);
#6659=ORIENTED_EDGE('',*,*,#5205,.T.);
#6660=ORIENTED_EDGE('',*,*,#5208,.F.);
#6661=ORIENTED_EDGE('',*,*,#5209,.F.);
#6662=ORIENTED_EDGE('',*,*,#5210,.T.);
#6663=ORIENTED_EDGE('',*,*,#5207,.T.);
#6664=ORIENTED_EDGE('',*,*,#5210,.F.);
#6665=ORIENTED_EDGE('',*,*,#5209,.T.);
#6666=ORIENTED_EDGE('',*,*,#5211,.F.);
#6667=ORIENTED_EDGE('',*,*,#5212,.F.);
#6668=ORIENTED_EDGE('',*,*,#5213,.T.);
#6669=ORIENTED_EDGE('',*,*,#5211,.T.);
#6670=ORIENTED_EDGE('',*,*,#5213,.F.);
#6671=ORIENTED_EDGE('',*,*,#5203,.T.);
#6672=ORIENTED_EDGE('',*,*,#5214,.T.);
#6673=ORIENTED_EDGE('',*,*,#5212,.T.);
#6674=ORIENTED_EDGE('',*,*,#5214,.F.);
#6675=ORIENTED_EDGE('',*,*,#5215,.F.);
#6676=ORIENTED_EDGE('',*,*,#5216,.F.);
#6677=ORIENTED_EDGE('',*,*,#5217,.T.);
#6678=ORIENTED_EDGE('',*,*,#5218,.F.);
#6679=ORIENTED_EDGE('',*,*,#5219,.F.);
#6680=ORIENTED_EDGE('',*,*,#5217,.F.);
#6681=ORIENTED_EDGE('',*,*,#5218,.T.);
#6682=ORIENTED_EDGE('',*,*,#5219,.T.);
#6683=ORIENTED_EDGE('',*,*,#5220,.T.);
#6684=ORIENTED_EDGE('',*,*,#5221,.T.);
#6685=ORIENTED_EDGE('',*,*,#5220,.F.);
#6686=ORIENTED_EDGE('',*,*,#5222,.T.);
#6687=ORIENTED_EDGE('',*,*,#5223,.T.);
#6688=ORIENTED_EDGE('',*,*,#5224,.F.);
#6689=ORIENTED_EDGE('',*,*,#5223,.F.);
#6690=ORIENTED_EDGE('',*,*,#5224,.T.);
#6691=ORIENTED_EDGE('',*,*,#5225,.T.);
#6692=ORIENTED_EDGE('',*,*,#5226,.F.);
#6693=ORIENTED_EDGE('',*,*,#5225,.F.);
#6694=ORIENTED_EDGE('',*,*,#5221,.F.);
#6695=ORIENTED_EDGE('',*,*,#5226,.T.);
#6696=ORIENTED_EDGE('',*,*,#5227,.F.);
#6697=ORIENTED_EDGE('',*,*,#5228,.T.);
#6698=ORIENTED_EDGE('',*,*,#5215,.T.);
#6699=ORIENTED_EDGE('',*,*,#5216,.T.);
#6700=ORIENTED_EDGE('',*,*,#5228,.F.);
#6701=ORIENTED_EDGE('',*,*,#5227,.T.);
#6702=ORIENTED_EDGE('',*,*,#5229,.F.);
#6703=ORIENTED_EDGE('',*,*,#5229,.T.);
#6704=ORIENTED_EDGE('',*,*,#5230,.T.);
#6705=ORIENTED_EDGE('',*,*,#5222,.F.);
#6706=ORIENTED_EDGE('',*,*,#5230,.F.);
#6707=ORIENTED_EDGE('',*,*,#5231,.F.);
#6708=ORIENTED_EDGE('',*,*,#5232,.F.);
#6709=ORIENTED_EDGE('',*,*,#5233,.T.);
#6710=ORIENTED_EDGE('',*,*,#5234,.F.);
#6711=ORIENTED_EDGE('',*,*,#5235,.F.);
#6712=ORIENTED_EDGE('',*,*,#5233,.F.);
#6713=ORIENTED_EDGE('',*,*,#5236,.T.);
#6714=ORIENTED_EDGE('',*,*,#5237,.T.);
#6715=ORIENTED_EDGE('',*,*,#5234,.T.);
#6716=ORIENTED_EDGE('',*,*,#5235,.T.);
#6717=ORIENTED_EDGE('',*,*,#5237,.F.);
#6718=ORIENTED_EDGE('',*,*,#5238,.F.);
#6719=ORIENTED_EDGE('',*,*,#5239,.T.);
#6720=ORIENTED_EDGE('',*,*,#5240,.F.);
#6721=ORIENTED_EDGE('',*,*,#5241,.T.);
#6722=ORIENTED_EDGE('',*,*,#5238,.T.);
#6723=ORIENTED_EDGE('',*,*,#5241,.F.);
#6724=ORIENTED_EDGE('',*,*,#5242,.F.);
#6725=ORIENTED_EDGE('',*,*,#5243,.T.);
#6726=ORIENTED_EDGE('',*,*,#5240,.T.);
#6727=ORIENTED_EDGE('',*,*,#5243,.F.);
#6728=ORIENTED_EDGE('',*,*,#5244,.F.);
#6729=ORIENTED_EDGE('',*,*,#5245,.T.);
#6730=ORIENTED_EDGE('',*,*,#5242,.T.);
#6731=ORIENTED_EDGE('',*,*,#5245,.F.);
#6732=ORIENTED_EDGE('',*,*,#5244,.T.);
#6733=ORIENTED_EDGE('',*,*,#5236,.F.);
#6734=ORIENTED_EDGE('',*,*,#5231,.T.);
#6735=ORIENTED_EDGE('',*,*,#5232,.T.);
#6736=ORIENTED_EDGE('',*,*,#5246,.T.);
#6737=ORIENTED_EDGE('',*,*,#5239,.F.);
#6738=ORIENTED_EDGE('',*,*,#5246,.F.);
#6739=ORIENTED_EDGE('',*,*,#5247,.T.);
#6740=ORIENTED_EDGE('',*,*,#5247,.F.);
#6741=ORIENTED_EDGE('',*,*,#5248,.T.);
#6742=ORIENTED_EDGE('',*,*,#5248,.F.);
#6743=ORIENTED_EDGE('',*,*,#5249,.T.);
#6744=ORIENTED_EDGE('',*,*,#5249,.F.);
#6745=ORIENTED_EDGE('',*,*,#5250,.T.);
#6746=ORIENTED_EDGE('',*,*,#5250,.F.);
#6747=ORIENTED_EDGE('',*,*,#5251,.T.);
#6748=ORIENTED_EDGE('',*,*,#5251,.F.);
#6749=ORIENTED_EDGE('',*,*,#5252,.T.);
#6750=ORIENTED_EDGE('',*,*,#5252,.F.);
#6751=ORIENTED_EDGE('',*,*,#5253,.T.);
#6752=ORIENTED_EDGE('',*,*,#5253,.F.);
#6753=ORIENTED_EDGE('',*,*,#5254,.T.);
#6754=ORIENTED_EDGE('',*,*,#5254,.F.);
#6755=ORIENTED_EDGE('',*,*,#5255,.F.);
#6756=ORIENTED_EDGE('',*,*,#5256,.F.);
#6757=ORIENTED_EDGE('',*,*,#5257,.F.);
#6758=ORIENTED_EDGE('',*,*,#5258,.F.);
#6759=ORIENTED_EDGE('',*,*,#5257,.T.);
#6760=ORIENTED_EDGE('',*,*,#5259,.F.);
#6761=ORIENTED_EDGE('',*,*,#5260,.T.);
#6762=ORIENTED_EDGE('',*,*,#5261,.F.);
#6763=ORIENTED_EDGE('',*,*,#5262,.T.);
#6764=ORIENTED_EDGE('',*,*,#5263,.F.);
#6765=ORIENTED_EDGE('',*,*,#5264,.T.);
#6766=ORIENTED_EDGE('',*,*,#5265,.T.);
#6767=ORIENTED_EDGE('',*,*,#5266,.F.);
#6768=ORIENTED_EDGE('',*,*,#5265,.F.);
#6769=ORIENTED_EDGE('',*,*,#5267,.T.);
#6770=ORIENTED_EDGE('',*,*,#5268,.F.);
#6771=ORIENTED_EDGE('',*,*,#5269,.T.);
#6772=ORIENTED_EDGE('',*,*,#5270,.F.);
#6773=ORIENTED_EDGE('',*,*,#5271,.T.);
#6774=ORIENTED_EDGE('',*,*,#5272,.F.);
#6775=ORIENTED_EDGE('',*,*,#5273,.T.);
#6776=ORIENTED_EDGE('',*,*,#5274,.F.);
#6777=ORIENTED_EDGE('',*,*,#5275,.T.);
#6778=ORIENTED_EDGE('',*,*,#5276,.F.);
#6779=ORIENTED_EDGE('',*,*,#5256,.T.);
#6780=ORIENTED_EDGE('',*,*,#5277,.T.);
#6781=ORIENTED_EDGE('',*,*,#5278,.T.);
#6782=ORIENTED_EDGE('',*,*,#5259,.T.);
#6783=ORIENTED_EDGE('',*,*,#5279,.F.);
#6784=ORIENTED_EDGE('',*,*,#5280,.F.);
#6785=ORIENTED_EDGE('',*,*,#5260,.F.);
#6786=ORIENTED_EDGE('',*,*,#5278,.F.);
#6787=ORIENTED_EDGE('',*,*,#5280,.T.);
#6788=ORIENTED_EDGE('',*,*,#5281,.T.);
#6789=ORIENTED_EDGE('',*,*,#5282,.T.);
#6790=ORIENTED_EDGE('',*,*,#5261,.T.);
#6791=ORIENTED_EDGE('',*,*,#5283,.F.);
#6792=ORIENTED_EDGE('',*,*,#5284,.F.);
#6793=ORIENTED_EDGE('',*,*,#5262,.F.);
#6794=ORIENTED_EDGE('',*,*,#5282,.F.);
#6795=ORIENTED_EDGE('',*,*,#5284,.T.);
#6796=ORIENTED_EDGE('',*,*,#5285,.T.);
#6797=ORIENTED_EDGE('',*,*,#5286,.T.);
#6798=ORIENTED_EDGE('',*,*,#5263,.T.);
#6799=ORIENTED_EDGE('',*,*,#5287,.F.);
#6800=ORIENTED_EDGE('',*,*,#5288,.F.);
#6801=ORIENTED_EDGE('',*,*,#5267,.F.);
#6802=ORIENTED_EDGE('',*,*,#5264,.F.);
#6803=ORIENTED_EDGE('',*,*,#5286,.F.);
#6804=ORIENTED_EDGE('',*,*,#5289,.F.);
#6805=ORIENTED_EDGE('',*,*,#5288,.T.);
#6806=ORIENTED_EDGE('',*,*,#5290,.T.);
#6807=ORIENTED_EDGE('',*,*,#5291,.T.);
#6808=ORIENTED_EDGE('',*,*,#5268,.T.);
#6809=ORIENTED_EDGE('',*,*,#5292,.F.);
#6810=ORIENTED_EDGE('',*,*,#5293,.F.);
#6811=ORIENTED_EDGE('',*,*,#5269,.F.);
#6812=ORIENTED_EDGE('',*,*,#5291,.F.);
#6813=ORIENTED_EDGE('',*,*,#5293,.T.);
#6814=ORIENTED_EDGE('',*,*,#5294,.T.);
#6815=ORIENTED_EDGE('',*,*,#5295,.T.);
#6816=ORIENTED_EDGE('',*,*,#5270,.T.);
#6817=ORIENTED_EDGE('',*,*,#5296,.F.);
#6818=ORIENTED_EDGE('',*,*,#5297,.F.);
#6819=ORIENTED_EDGE('',*,*,#5271,.F.);
#6820=ORIENTED_EDGE('',*,*,#5295,.F.);
#6821=ORIENTED_EDGE('',*,*,#5297,.T.);
#6822=ORIENTED_EDGE('',*,*,#5298,.T.);
#6823=ORIENTED_EDGE('',*,*,#5299,.T.);
#6824=ORIENTED_EDGE('',*,*,#5272,.T.);
#6825=ORIENTED_EDGE('',*,*,#5273,.F.);
#6826=ORIENTED_EDGE('',*,*,#5299,.F.);
#6827=ORIENTED_EDGE('',*,*,#5300,.F.);
#6828=ORIENTED_EDGE('',*,*,#5301,.F.);
#6829=ORIENTED_EDGE('',*,*,#5302,.F.);
#6830=ORIENTED_EDGE('',*,*,#5303,.T.);
#6831=ORIENTED_EDGE('',*,*,#5289,.T.);
#6832=ORIENTED_EDGE('',*,*,#5285,.F.);
#6833=ORIENTED_EDGE('',*,*,#5283,.T.);
#6834=ORIENTED_EDGE('',*,*,#5281,.F.);
#6835=ORIENTED_EDGE('',*,*,#5279,.T.);
#6836=ORIENTED_EDGE('',*,*,#5277,.F.);
#6837=ORIENTED_EDGE('',*,*,#5255,.T.);
#6838=ORIENTED_EDGE('',*,*,#5304,.F.);
#6839=ORIENTED_EDGE('',*,*,#5305,.T.);
#6840=ORIENTED_EDGE('',*,*,#5306,.F.);
#6841=ORIENTED_EDGE('',*,*,#5300,.T.);
#6842=ORIENTED_EDGE('',*,*,#5298,.F.);
#6843=ORIENTED_EDGE('',*,*,#5296,.T.);
#6844=ORIENTED_EDGE('',*,*,#5294,.F.);
#6845=ORIENTED_EDGE('',*,*,#5292,.T.);
#6846=ORIENTED_EDGE('',*,*,#5290,.F.);
#6847=ORIENTED_EDGE('',*,*,#5287,.T.);
#6848=ORIENTED_EDGE('',*,*,#5303,.F.);
#6849=ORIENTED_EDGE('',*,*,#5258,.T.);
#6850=ORIENTED_EDGE('',*,*,#5276,.T.);
#6851=ORIENTED_EDGE('',*,*,#5307,.T.);
#6852=ORIENTED_EDGE('',*,*,#5304,.T.);
#6853=ORIENTED_EDGE('',*,*,#5275,.F.);
#6854=ORIENTED_EDGE('',*,*,#5308,.F.);
#6855=ORIENTED_EDGE('',*,*,#5305,.F.);
#6856=ORIENTED_EDGE('',*,*,#5307,.F.);
#6857=ORIENTED_EDGE('',*,*,#5266,.T.);
#6858=ORIENTED_EDGE('',*,*,#5302,.T.);
#6859=ORIENTED_EDGE('',*,*,#5301,.T.);
#6860=ORIENTED_EDGE('',*,*,#5306,.T.);
#6861=ORIENTED_EDGE('',*,*,#5308,.T.);
#6862=ORIENTED_EDGE('',*,*,#5274,.T.);
#6863=ORIENTED_EDGE('',*,*,#5309,.F.);
#6864=ORIENTED_EDGE('',*,*,#5310,.T.);
#6865=ORIENTED_EDGE('',*,*,#5311,.F.);
#6866=ORIENTED_EDGE('',*,*,#5312,.T.);
#6867=ORIENTED_EDGE('',*,*,#5309,.T.);
#6868=ORIENTED_EDGE('',*,*,#5312,.F.);
#6869=ORIENTED_EDGE('',*,*,#5311,.T.);
#6870=ORIENTED_EDGE('',*,*,#5313,.F.);
#6871=ORIENTED_EDGE('',*,*,#5313,.T.);
#6872=ORIENTED_EDGE('',*,*,#5314,.T.);
#6873=ORIENTED_EDGE('',*,*,#5310,.F.);
#6874=ORIENTED_EDGE('',*,*,#5314,.F.);
#6875=ORIENTED_EDGE('',*,*,#5315,.F.);
#6876=ORIENTED_EDGE('',*,*,#5316,.T.);
#6877=ORIENTED_EDGE('',*,*,#5317,.F.);
#6878=ORIENTED_EDGE('',*,*,#5318,.T.);
#6879=ORIENTED_EDGE('',*,*,#5315,.T.);
#6880=ORIENTED_EDGE('',*,*,#5318,.F.);
#6881=ORIENTED_EDGE('',*,*,#5317,.T.);
#6882=ORIENTED_EDGE('',*,*,#5319,.F.);
#6883=ORIENTED_EDGE('',*,*,#5319,.T.);
#6884=ORIENTED_EDGE('',*,*,#5320,.T.);
#6885=ORIENTED_EDGE('',*,*,#5316,.F.);
#6886=ORIENTED_EDGE('',*,*,#5320,.F.);
#6887=ORIENTED_EDGE('',*,*,#5321,.F.);
#6888=ORIENTED_EDGE('',*,*,#5322,.T.);
#6889=ORIENTED_EDGE('',*,*,#5323,.T.);
#6890=ORIENTED_EDGE('',*,*,#5324,.T.);
#6891=ORIENTED_EDGE('',*,*,#5323,.F.);
#6892=ORIENTED_EDGE('',*,*,#5321,.T.);
#6893=ORIENTED_EDGE('',*,*,#5325,.T.);
#6894=ORIENTED_EDGE('',*,*,#5322,.F.);
#6895=ORIENTED_EDGE('',*,*,#5325,.F.);
#6896=ORIENTED_EDGE('',*,*,#5324,.F.);
#6897=ORIENTED_EDGE('',*,*,#5326,.F.);
#6898=ORIENTED_EDGE('',*,*,#5327,.T.);
#6899=ORIENTED_EDGE('',*,*,#5328,.T.);
#6900=ORIENTED_EDGE('',*,*,#5329,.F.);
#6901=ORIENTED_EDGE('',*,*,#5330,.F.);
#6902=ORIENTED_EDGE('',*,*,#5331,.T.);
#6903=ORIENTED_EDGE('',*,*,#5332,.T.);
#6904=ORIENTED_EDGE('',*,*,#5327,.F.);
#6905=ORIENTED_EDGE('',*,*,#5333,.F.);
#6906=ORIENTED_EDGE('',*,*,#5334,.T.);
#6907=ORIENTED_EDGE('',*,*,#5335,.T.);
#6908=ORIENTED_EDGE('',*,*,#5331,.F.);
#6909=ORIENTED_EDGE('',*,*,#5336,.F.);
#6910=ORIENTED_EDGE('',*,*,#5337,.T.);
#6911=ORIENTED_EDGE('',*,*,#5338,.T.);
#6912=ORIENTED_EDGE('',*,*,#5334,.F.);
#6913=ORIENTED_EDGE('',*,*,#5339,.F.);
#6914=ORIENTED_EDGE('',*,*,#5340,.T.);
#6915=ORIENTED_EDGE('',*,*,#5341,.T.);
#6916=ORIENTED_EDGE('',*,*,#5337,.F.);
#6917=ORIENTED_EDGE('',*,*,#5342,.F.);
#6918=ORIENTED_EDGE('',*,*,#5329,.T.);
#6919=ORIENTED_EDGE('',*,*,#5343,.T.);
#6920=ORIENTED_EDGE('',*,*,#5340,.F.);
#6921=ORIENTED_EDGE('',*,*,#5343,.F.);
#6922=ORIENTED_EDGE('',*,*,#5328,.F.);
#6923=ORIENTED_EDGE('',*,*,#5332,.F.);
#6924=ORIENTED_EDGE('',*,*,#5335,.F.);
#6925=ORIENTED_EDGE('',*,*,#5338,.F.);
#6926=ORIENTED_EDGE('',*,*,#5341,.F.);
#6927=ORIENTED_EDGE('',*,*,#5344,.F.);
#6928=ORIENTED_EDGE('',*,*,#5326,.T.);
#6929=ORIENTED_EDGE('',*,*,#5342,.T.);
#6930=ORIENTED_EDGE('',*,*,#5339,.T.);
#6931=ORIENTED_EDGE('',*,*,#5336,.T.);
#6932=ORIENTED_EDGE('',*,*,#5333,.T.);
#6933=ORIENTED_EDGE('',*,*,#5330,.T.);
#6934=ORIENTED_EDGE('',*,*,#5345,.F.);
#6935=ORIENTED_EDGE('',*,*,#5346,.T.);
#6936=ORIENTED_EDGE('',*,*,#5344,.T.);
#6937=ORIENTED_EDGE('',*,*,#5346,.F.);
#6938=ORIENTED_EDGE('',*,*,#5347,.F.);
#6939=ORIENTED_EDGE('',*,*,#5348,.T.);
#6940=ORIENTED_EDGE('',*,*,#5345,.T.);
#6941=ORIENTED_EDGE('',*,*,#5348,.F.);
#6942=ORIENTED_EDGE('',*,*,#5349,.F.);
#6943=ORIENTED_EDGE('',*,*,#5350,.T.);
#6944=ORIENTED_EDGE('',*,*,#5347,.T.);
#6945=ORIENTED_EDGE('',*,*,#5350,.F.);
#6946=ORIENTED_EDGE('',*,*,#5349,.T.);
#6947=ORIENTED_EDGE('',*,*,#5351,.F.);
#6948=ORIENTED_EDGE('',*,*,#5352,.T.);
#6949=ORIENTED_EDGE('',*,*,#5353,.F.);
#6950=ORIENTED_EDGE('',*,*,#5352,.F.);
#6951=ORIENTED_EDGE('',*,*,#5354,.F.);
#6952=ORIENTED_EDGE('',*,*,#5355,.T.);
#6953=ORIENTED_EDGE('',*,*,#5356,.F.);
#6954=ORIENTED_EDGE('',*,*,#5355,.F.);
#6955=ORIENTED_EDGE('',*,*,#5357,.F.);
#6956=ORIENTED_EDGE('',*,*,#5358,.T.);
#6957=ORIENTED_EDGE('',*,*,#5359,.F.);
#6958=ORIENTED_EDGE('',*,*,#5358,.F.);
#6959=ORIENTED_EDGE('',*,*,#5360,.F.);
#6960=ORIENTED_EDGE('',*,*,#5361,.T.);
#6961=ORIENTED_EDGE('',*,*,#5362,.F.);
#6962=ORIENTED_EDGE('',*,*,#5363,.F.);
#6963=ORIENTED_EDGE('',*,*,#5360,.T.);
#6964=ORIENTED_EDGE('',*,*,#5364,.F.);
#6965=ORIENTED_EDGE('',*,*,#5365,.F.);
#6966=ORIENTED_EDGE('',*,*,#5366,.F.);
#6967=ORIENTED_EDGE('',*,*,#5363,.T.);
#6968=ORIENTED_EDGE('',*,*,#5367,.T.);
#6969=ORIENTED_EDGE('',*,*,#5368,.T.);
#6970=ORIENTED_EDGE('',*,*,#5369,.T.);
#6971=ORIENTED_EDGE('',*,*,#5370,.T.);
#6972=ORIENTED_EDGE('',*,*,#5371,.T.);
#6973=ORIENTED_EDGE('',*,*,#5372,.T.);
#6974=ORIENTED_EDGE('',*,*,#5373,.T.);
#6975=ORIENTED_EDGE('',*,*,#5374,.T.);
#6976=ORIENTED_EDGE('',*,*,#5375,.T.);
#6977=ORIENTED_EDGE('',*,*,#5376,.T.);
#6978=ORIENTED_EDGE('',*,*,#5364,.T.);
#6979=ORIENTED_EDGE('',*,*,#5353,.T.);
#6980=ORIENTED_EDGE('',*,*,#5356,.T.);
#6981=ORIENTED_EDGE('',*,*,#5359,.T.);
#6982=ORIENTED_EDGE('',*,*,#5362,.T.);
#6983=ORIENTED_EDGE('',*,*,#5377,.F.);
#6984=ORIENTED_EDGE('',*,*,#5378,.F.);
#6985=ORIENTED_EDGE('',*,*,#5367,.F.);
#6986=ORIENTED_EDGE('',*,*,#5365,.T.);
#6987=ORIENTED_EDGE('',*,*,#5376,.F.);
#6988=ORIENTED_EDGE('',*,*,#5379,.T.);
#6989=ORIENTED_EDGE('',*,*,#5380,.T.);
#6990=ORIENTED_EDGE('',*,*,#5378,.T.);
#6991=ORIENTED_EDGE('',*,*,#5381,.T.);
#6992=ORIENTED_EDGE('',*,*,#5382,.T.);
#6993=ORIENTED_EDGE('',*,*,#5368,.F.);
#6994=ORIENTED_EDGE('',*,*,#5383,.F.);
#6995=ORIENTED_EDGE('',*,*,#5370,.F.);
#6996=ORIENTED_EDGE('',*,*,#5384,.F.);
#6997=ORIENTED_EDGE('',*,*,#5385,.T.);
#6998=ORIENTED_EDGE('',*,*,#5383,.T.);
#6999=ORIENTED_EDGE('',*,*,#5386,.F.);
#7000=ORIENTED_EDGE('',*,*,#5387,.F.);
#7001=ORIENTED_EDGE('',*,*,#5371,.F.);
#7002=ORIENTED_EDGE('',*,*,#5366,.T.);
#7003=ORIENTED_EDGE('',*,*,#5380,.F.);
#7004=ORIENTED_EDGE('',*,*,#5388,.T.);
#7005=ORIENTED_EDGE('',*,*,#5389,.F.);
#7006=ORIENTED_EDGE('',*,*,#5390,.T.);
#7007=ORIENTED_EDGE('',*,*,#5391,.F.);
#7008=ORIENTED_EDGE('',*,*,#5386,.T.);
#7009=ORIENTED_EDGE('',*,*,#5385,.F.);
#7010=ORIENTED_EDGE('',*,*,#5392,.T.);
#7011=ORIENTED_EDGE('',*,*,#5381,.F.);
#7012=ORIENTED_EDGE('',*,*,#5377,.T.);
#7013=ORIENTED_EDGE('',*,*,#5361,.F.);
#7014=ORIENTED_EDGE('',*,*,#5351,.T.);
#7015=ORIENTED_EDGE('',*,*,#5354,.T.);
#7016=ORIENTED_EDGE('',*,*,#5357,.T.);
#7017=ORIENTED_EDGE('',*,*,#5393,.T.);
#7018=ORIENTED_EDGE('',*,*,#5384,.T.);
#7019=ORIENTED_EDGE('',*,*,#5369,.F.);
#7020=ORIENTED_EDGE('',*,*,#5382,.F.);
#7021=ORIENTED_EDGE('',*,*,#5392,.F.);
#7022=ORIENTED_EDGE('',*,*,#5394,.F.);
#7023=ORIENTED_EDGE('',*,*,#5389,.T.);
#7024=ORIENTED_EDGE('',*,*,#5395,.F.);
#7025=ORIENTED_EDGE('',*,*,#5374,.F.);
#7026=ORIENTED_EDGE('',*,*,#5394,.T.);
#7027=ORIENTED_EDGE('',*,*,#5373,.F.);
#7028=ORIENTED_EDGE('',*,*,#5396,.F.);
#7029=ORIENTED_EDGE('',*,*,#5390,.F.);
#7030=ORIENTED_EDGE('',*,*,#5395,.T.);
#7031=ORIENTED_EDGE('',*,*,#5388,.F.);
#7032=ORIENTED_EDGE('',*,*,#5379,.F.);
#7033=ORIENTED_EDGE('',*,*,#5375,.F.);
#7034=ORIENTED_EDGE('',*,*,#5387,.T.);
#7035=ORIENTED_EDGE('',*,*,#5391,.T.);
#7036=ORIENTED_EDGE('',*,*,#5396,.T.);
#7037=ORIENTED_EDGE('',*,*,#5372,.F.);
#7038=ORIENTED_EDGE('',*,*,#5397,.F.);
#7039=ORIENTED_EDGE('',*,*,#5398,.F.);
#7040=ORIENTED_EDGE('',*,*,#5393,.F.);
#7041=ORIENTED_EDGE('',*,*,#5399,.T.);
#7042=ORIENTED_EDGE('',*,*,#5397,.T.);
#7043=ORIENTED_EDGE('',*,*,#5399,.F.);
#7044=ORIENTED_EDGE('',*,*,#5398,.T.);
#7045=ORIENTED_EDGE('',*,*,#5400,.T.);
#7046=ORIENTED_EDGE('',*,*,#5401,.T.);
#7047=ORIENTED_EDGE('',*,*,#5400,.F.);
#7048=ORIENTED_EDGE('',*,*,#5401,.F.);
#7049=ORIENTED_EDGE('',*,*,#5402,.F.);
#7050=ORIENTED_EDGE('',*,*,#5403,.T.);
#7051=ORIENTED_EDGE('',*,*,#5404,.T.);
#7052=ORIENTED_EDGE('',*,*,#5403,.F.);
#7053=ORIENTED_EDGE('',*,*,#5404,.F.);
#7054=ORIENTED_EDGE('',*,*,#5405,.F.);
#7055=ORIENTED_EDGE('',*,*,#5406,.T.);
#7056=ORIENTED_EDGE('',*,*,#5407,.T.);
#7057=ORIENTED_EDGE('',*,*,#5406,.F.);
#7058=ORIENTED_EDGE('',*,*,#5405,.T.);
#7059=ORIENTED_EDGE('',*,*,#5407,.F.);
#7060=ORIENTED_EDGE('',*,*,#5402,.T.);
#7061=ORIENTED_EDGE('',*,*,#5408,.F.);
#7062=ORIENTED_EDGE('',*,*,#5409,.T.);
#7063=ORIENTED_EDGE('',*,*,#5410,.T.);
#7064=ORIENTED_EDGE('',*,*,#5409,.F.);
#7065=ORIENTED_EDGE('',*,*,#5411,.F.);
#7066=ORIENTED_EDGE('',*,*,#5412,.T.);
#7067=ORIENTED_EDGE('',*,*,#5413,.T.);
#7068=ORIENTED_EDGE('',*,*,#5412,.F.);
#7069=ORIENTED_EDGE('',*,*,#5411,.T.);
#7070=ORIENTED_EDGE('',*,*,#5408,.T.);
#7071=ORIENTED_EDGE('',*,*,#5413,.F.);
#7072=ORIENTED_EDGE('',*,*,#5410,.F.);
#7073=ORIENTED_EDGE('',*,*,#5414,.F.);
#7074=ORIENTED_EDGE('',*,*,#5415,.T.);
#7075=ORIENTED_EDGE('',*,*,#5416,.F.);
#7076=ORIENTED_EDGE('',*,*,#5417,.F.);
#7077=ORIENTED_EDGE('',*,*,#5418,.F.);
#7078=ORIENTED_EDGE('',*,*,#5419,.T.);
#7079=ORIENTED_EDGE('',*,*,#5420,.F.);
#7080=ORIENTED_EDGE('',*,*,#5421,.F.);
#7081=ORIENTED_EDGE('',*,*,#5419,.F.);
#7082=ORIENTED_EDGE('',*,*,#5422,.F.);
#7083=ORIENTED_EDGE('',*,*,#5415,.F.);
#7084=ORIENTED_EDGE('',*,*,#5423,.F.);
#7085=ORIENTED_EDGE('',*,*,#5417,.T.);
#7086=ORIENTED_EDGE('',*,*,#5424,.F.);
#7087=ORIENTED_EDGE('',*,*,#5425,.T.);
#7088=ORIENTED_EDGE('',*,*,#5426,.T.);
#7089=ORIENTED_EDGE('',*,*,#5425,.F.);
#7090=ORIENTED_EDGE('',*,*,#5422,.T.);
#7091=ORIENTED_EDGE('',*,*,#5418,.T.);
#7092=ORIENTED_EDGE('',*,*,#5423,.T.);
#7093=ORIENTED_EDGE('',*,*,#5416,.T.);
#7094=ORIENTED_EDGE('',*,*,#5414,.T.);
#7095=ORIENTED_EDGE('',*,*,#5427,.F.);
#7096=ORIENTED_EDGE('',*,*,#5428,.T.);
#7097=ORIENTED_EDGE('',*,*,#5429,.T.);
#7098=ORIENTED_EDGE('',*,*,#5428,.F.);
#7099=ORIENTED_EDGE('',*,*,#5420,.T.);
#7100=ORIENTED_EDGE('',*,*,#5421,.T.);
#7101=ORIENTED_EDGE('',*,*,#5427,.T.);
#7102=ORIENTED_EDGE('',*,*,#5424,.T.);
#7103=ORIENTED_EDGE('',*,*,#5429,.F.);
#7104=ORIENTED_EDGE('',*,*,#5426,.F.);
#7105=ORIENTED_EDGE('',*,*,#5430,.F.);
#7106=ORIENTED_EDGE('',*,*,#5431,.T.);
#7107=ORIENTED_EDGE('',*,*,#5432,.F.);
#7108=ORIENTED_EDGE('',*,*,#5431,.F.);
#7109=ORIENTED_EDGE('',*,*,#5430,.T.);
#7110=ORIENTED_EDGE('',*,*,#5433,.T.);
#7111=ORIENTED_EDGE('',*,*,#5434,.F.);
#7112=ORIENTED_EDGE('',*,*,#5435,.F.);
#7113=ORIENTED_EDGE('',*,*,#5436,.F.);
#7114=ORIENTED_EDGE('',*,*,#5433,.F.);
#7115=ORIENTED_EDGE('',*,*,#5437,.T.);
#7116=ORIENTED_EDGE('',*,*,#5435,.T.);
#7117=ORIENTED_EDGE('',*,*,#5437,.F.);
#7118=ORIENTED_EDGE('',*,*,#5436,.T.);
#7119=ORIENTED_EDGE('',*,*,#5438,.T.);
#7120=ORIENTED_EDGE('',*,*,#5439,.T.);
#7121=ORIENTED_EDGE('',*,*,#5438,.F.);
#7122=ORIENTED_EDGE('',*,*,#5440,.F.);
#7123=ORIENTED_EDGE('',*,*,#5441,.T.);
#7124=ORIENTED_EDGE('',*,*,#5434,.T.);
#7125=ORIENTED_EDGE('',*,*,#5441,.F.);
#7126=ORIENTED_EDGE('',*,*,#5440,.T.);
#7127=ORIENTED_EDGE('',*,*,#5432,.T.);
#7128=ORIENTED_EDGE('',*,*,#5439,.F.);
#7129=ORIENTED_EDGE('',*,*,#5442,.F.);
#7130=ORIENTED_EDGE('',*,*,#5443,.T.);
#7131=ORIENTED_EDGE('',*,*,#5444,.T.);
#7132=ORIENTED_EDGE('',*,*,#5443,.F.);
#7133=ORIENTED_EDGE('',*,*,#5445,.F.);
#7134=ORIENTED_EDGE('',*,*,#5446,.T.);
#7135=ORIENTED_EDGE('',*,*,#5447,.T.);
#7136=ORIENTED_EDGE('',*,*,#5446,.F.);
#7137=ORIENTED_EDGE('',*,*,#5445,.T.);
#7138=ORIENTED_EDGE('',*,*,#5442,.T.);
#7139=ORIENTED_EDGE('',*,*,#5447,.F.);
#7140=ORIENTED_EDGE('',*,*,#5444,.F.);
#7141=ORIENTED_EDGE('',*,*,#5448,.F.);
#7142=ORIENTED_EDGE('',*,*,#5449,.T.);
#7143=ORIENTED_EDGE('',*,*,#5450,.T.);
#7144=ORIENTED_EDGE('',*,*,#5449,.F.);
#7145=ORIENTED_EDGE('',*,*,#5451,.F.);
#7146=ORIENTED_EDGE('',*,*,#5452,.T.);
#7147=ORIENTED_EDGE('',*,*,#5453,.T.);
#7148=ORIENTED_EDGE('',*,*,#5452,.F.);
#7149=ORIENTED_EDGE('',*,*,#5451,.T.);
#7150=ORIENTED_EDGE('',*,*,#5448,.T.);
#7151=ORIENTED_EDGE('',*,*,#5453,.F.);
#7152=ORIENTED_EDGE('',*,*,#5450,.F.);
#7153=ORIENTED_EDGE('',*,*,#5454,.F.);
#7154=ORIENTED_EDGE('',*,*,#5455,.T.);
#7155=ORIENTED_EDGE('',*,*,#5456,.T.);
#7156=ORIENTED_EDGE('',*,*,#5455,.F.);
#7157=ORIENTED_EDGE('',*,*,#5457,.F.);
#7158=ORIENTED_EDGE('',*,*,#5458,.T.);
#7159=ORIENTED_EDGE('',*,*,#5459,.T.);
#7160=ORIENTED_EDGE('',*,*,#5458,.F.);
#7161=ORIENTED_EDGE('',*,*,#5457,.T.);
#7162=ORIENTED_EDGE('',*,*,#5454,.T.);
#7163=ORIENTED_EDGE('',*,*,#5459,.F.);
#7164=ORIENTED_EDGE('',*,*,#5456,.F.);
#7165=ORIENTED_EDGE('',*,*,#5460,.F.);
#7166=ORIENTED_EDGE('',*,*,#5461,.T.);
#7167=ORIENTED_EDGE('',*,*,#5462,.F.);
#7168=ORIENTED_EDGE('',*,*,#5461,.F.);
#7169=ORIENTED_EDGE('',*,*,#5460,.T.);
#7170=ORIENTED_EDGE('',*,*,#5463,.T.);
#7171=ORIENTED_EDGE('',*,*,#5464,.F.);
#7172=ORIENTED_EDGE('',*,*,#5465,.F.);
#7173=ORIENTED_EDGE('',*,*,#5466,.F.);
#7174=ORIENTED_EDGE('',*,*,#5463,.F.);
#7175=ORIENTED_EDGE('',*,*,#5467,.T.);
#7176=ORIENTED_EDGE('',*,*,#5465,.T.);
#7177=ORIENTED_EDGE('',*,*,#5467,.F.);
#7178=ORIENTED_EDGE('',*,*,#5466,.T.);
#7179=ORIENTED_EDGE('',*,*,#5468,.T.);
#7180=ORIENTED_EDGE('',*,*,#5469,.T.);
#7181=ORIENTED_EDGE('',*,*,#5468,.F.);
#7182=ORIENTED_EDGE('',*,*,#5470,.F.);
#7183=ORIENTED_EDGE('',*,*,#5471,.T.);
#7184=ORIENTED_EDGE('',*,*,#5464,.T.);
#7185=ORIENTED_EDGE('',*,*,#5471,.F.);
#7186=ORIENTED_EDGE('',*,*,#5470,.T.);
#7187=ORIENTED_EDGE('',*,*,#5462,.T.);
#7188=ORIENTED_EDGE('',*,*,#5469,.F.);
#7189=ORIENTED_EDGE('',*,*,#5472,.F.);
#7190=ORIENTED_EDGE('',*,*,#5473,.T.);
#7191=ORIENTED_EDGE('',*,*,#5474,.T.);
#7192=ORIENTED_EDGE('',*,*,#5473,.F.);
#7193=ORIENTED_EDGE('',*,*,#5475,.F.);
#7194=ORIENTED_EDGE('',*,*,#5476,.T.);
#7195=ORIENTED_EDGE('',*,*,#5477,.T.);
#7196=ORIENTED_EDGE('',*,*,#5476,.F.);
#7197=ORIENTED_EDGE('',*,*,#5475,.T.);
#7198=ORIENTED_EDGE('',*,*,#5472,.T.);
#7199=ORIENTED_EDGE('',*,*,#5477,.F.);
#7200=ORIENTED_EDGE('',*,*,#5474,.F.);
#7201=ORIENTED_EDGE('',*,*,#5478,.F.);
#7202=ORIENTED_EDGE('',*,*,#5479,.T.);
#7203=ORIENTED_EDGE('',*,*,#5480,.T.);
#7204=ORIENTED_EDGE('',*,*,#5479,.F.);
#7205=ORIENTED_EDGE('',*,*,#5481,.F.);
#7206=ORIENTED_EDGE('',*,*,#5482,.T.);
#7207=ORIENTED_EDGE('',*,*,#5483,.T.);
#7208=ORIENTED_EDGE('',*,*,#5482,.F.);
#7209=ORIENTED_EDGE('',*,*,#5481,.T.);
#7210=ORIENTED_EDGE('',*,*,#5478,.T.);
#7211=ORIENTED_EDGE('',*,*,#5483,.F.);
#7212=ORIENTED_EDGE('',*,*,#5480,.F.);
#7213=ORIENTED_EDGE('',*,*,#5484,.F.);
#7214=ORIENTED_EDGE('',*,*,#5485,.T.);
#7215=ORIENTED_EDGE('',*,*,#5486,.T.);
#7216=ORIENTED_EDGE('',*,*,#5485,.F.);
#7217=ORIENTED_EDGE('',*,*,#5487,.F.);
#7218=ORIENTED_EDGE('',*,*,#5488,.T.);
#7219=ORIENTED_EDGE('',*,*,#5489,.T.);
#7220=ORIENTED_EDGE('',*,*,#5488,.F.);
#7221=ORIENTED_EDGE('',*,*,#5487,.T.);
#7222=ORIENTED_EDGE('',*,*,#5484,.T.);
#7223=ORIENTED_EDGE('',*,*,#5489,.F.);
#7224=ORIENTED_EDGE('',*,*,#5486,.F.);
#7225=ORIENTED_EDGE('',*,*,#5490,.F.);
#7226=ORIENTED_EDGE('',*,*,#5491,.F.);
#7227=ORIENTED_EDGE('',*,*,#5492,.T.);
#7228=ORIENTED_EDGE('',*,*,#5490,.T.);
#7229=ORIENTED_EDGE('',*,*,#5492,.F.);
#7230=ORIENTED_EDGE('',*,*,#5493,.F.);
#7231=ORIENTED_EDGE('',*,*,#5494,.T.);
#7232=ORIENTED_EDGE('',*,*,#5491,.T.);
#7233=ORIENTED_EDGE('',*,*,#5494,.F.);
#7234=ORIENTED_EDGE('',*,*,#5495,.F.);
#7235=ORIENTED_EDGE('',*,*,#5496,.T.);
#7236=ORIENTED_EDGE('',*,*,#5493,.T.);
#7237=ORIENTED_EDGE('',*,*,#5496,.F.);
#7238=ORIENTED_EDGE('',*,*,#5495,.T.);
#7239=ORIENTED_EDGE('',*,*,#5497,.F.);
#7240=ORIENTED_EDGE('',*,*,#5498,.F.);
#7241=ORIENTED_EDGE('',*,*,#5499,.T.);
#7242=ORIENTED_EDGE('',*,*,#5497,.T.);
#7243=ORIENTED_EDGE('',*,*,#5499,.F.);
#7244=ORIENTED_EDGE('',*,*,#5500,.F.);
#7245=ORIENTED_EDGE('',*,*,#5501,.T.);
#7246=ORIENTED_EDGE('',*,*,#5498,.T.);
#7247=ORIENTED_EDGE('',*,*,#5501,.F.);
#7248=ORIENTED_EDGE('',*,*,#5502,.F.);
#7249=ORIENTED_EDGE('',*,*,#5503,.T.);
#7250=ORIENTED_EDGE('',*,*,#5500,.T.);
#7251=ORIENTED_EDGE('',*,*,#5503,.F.);
#7252=ORIENTED_EDGE('',*,*,#5502,.T.);
#7253=ORIENTED_EDGE('',*,*,#5504,.T.);
#7254=ORIENTED_EDGE('',*,*,#5505,.T.);
#7255=ORIENTED_EDGE('',*,*,#5506,.T.);
#7256=ORIENTED_EDGE('',*,*,#5507,.F.);
#7257=ORIENTED_EDGE('',*,*,#5508,.T.);
#7258=ORIENTED_EDGE('',*,*,#5509,.T.);
#7259=ORIENTED_EDGE('',*,*,#5510,.T.);
#7260=ORIENTED_EDGE('',*,*,#5505,.F.);
#7261=ORIENTED_EDGE('',*,*,#5511,.T.);
#7262=ORIENTED_EDGE('',*,*,#5512,.T.);
#7263=ORIENTED_EDGE('',*,*,#5513,.T.);
#7264=ORIENTED_EDGE('',*,*,#5509,.F.);
#7265=ORIENTED_EDGE('',*,*,#5514,.T.);
#7266=ORIENTED_EDGE('',*,*,#5515,.T.);
#7267=ORIENTED_EDGE('',*,*,#5516,.T.);
#7268=ORIENTED_EDGE('',*,*,#5512,.F.);
#7269=ORIENTED_EDGE('',*,*,#5517,.T.);
#7270=ORIENTED_EDGE('',*,*,#5518,.T.);
#7271=ORIENTED_EDGE('',*,*,#5519,.T.);
#7272=ORIENTED_EDGE('',*,*,#5515,.F.);
#7273=ORIENTED_EDGE('',*,*,#5520,.T.);
#7274=ORIENTED_EDGE('',*,*,#5507,.T.);
#7275=ORIENTED_EDGE('',*,*,#5521,.T.);
#7276=ORIENTED_EDGE('',*,*,#5518,.F.);
#7277=ORIENTED_EDGE('',*,*,#5520,.F.);
#7278=ORIENTED_EDGE('',*,*,#5517,.F.);
#7279=ORIENTED_EDGE('',*,*,#5514,.F.);
#7280=ORIENTED_EDGE('',*,*,#5511,.F.);
#7281=ORIENTED_EDGE('',*,*,#5508,.F.);
#7282=ORIENTED_EDGE('',*,*,#5504,.F.);
#7283=ORIENTED_EDGE('',*,*,#5521,.F.);
#7284=ORIENTED_EDGE('',*,*,#5506,.F.);
#7285=ORIENTED_EDGE('',*,*,#5510,.F.);
#7286=ORIENTED_EDGE('',*,*,#5513,.F.);
#7287=ORIENTED_EDGE('',*,*,#5516,.F.);
#7288=ORIENTED_EDGE('',*,*,#5519,.F.);
#7289=ORIENTED_EDGE('',*,*,#5522,.F.);
#7290=ORIENTED_EDGE('',*,*,#5523,.F.);
#7291=ORIENTED_EDGE('',*,*,#5524,.T.);
#7292=ORIENTED_EDGE('',*,*,#5525,.T.);
#7293=ORIENTED_EDGE('',*,*,#5526,.F.);
#7294=ORIENTED_EDGE('',*,*,#5527,.F.);
#7295=ORIENTED_EDGE('',*,*,#5528,.T.);
#7296=ORIENTED_EDGE('',*,*,#5529,.T.);
#7297=ORIENTED_EDGE('',*,*,#5524,.F.);
#7298=ORIENTED_EDGE('',*,*,#5530,.F.);
#7299=ORIENTED_EDGE('',*,*,#5531,.T.);
#7300=ORIENTED_EDGE('',*,*,#5532,.T.);
#7301=ORIENTED_EDGE('',*,*,#5528,.F.);
#7302=ORIENTED_EDGE('',*,*,#5533,.F.);
#7303=ORIENTED_EDGE('',*,*,#5534,.T.);
#7304=ORIENTED_EDGE('',*,*,#5535,.T.);
#7305=ORIENTED_EDGE('',*,*,#5531,.F.);
#7306=ORIENTED_EDGE('',*,*,#5536,.F.);
#7307=ORIENTED_EDGE('',*,*,#5537,.T.);
#7308=ORIENTED_EDGE('',*,*,#5538,.T.);
#7309=ORIENTED_EDGE('',*,*,#5534,.F.);
#7310=ORIENTED_EDGE('',*,*,#5539,.F.);
#7311=ORIENTED_EDGE('',*,*,#5526,.T.);
#7312=ORIENTED_EDGE('',*,*,#5540,.T.);
#7313=ORIENTED_EDGE('',*,*,#5537,.F.);
#7314=ORIENTED_EDGE('',*,*,#5540,.F.);
#7315=ORIENTED_EDGE('',*,*,#5525,.F.);
#7316=ORIENTED_EDGE('',*,*,#5529,.F.);
#7317=ORIENTED_EDGE('',*,*,#5532,.F.);
#7318=ORIENTED_EDGE('',*,*,#5535,.F.);
#7319=ORIENTED_EDGE('',*,*,#5538,.F.);
#7320=ORIENTED_EDGE('',*,*,#5541,.F.);
#7321=ORIENTED_EDGE('',*,*,#5523,.T.);
#7322=ORIENTED_EDGE('',*,*,#5539,.T.);
#7323=ORIENTED_EDGE('',*,*,#5536,.T.);
#7324=ORIENTED_EDGE('',*,*,#5533,.T.);
#7325=ORIENTED_EDGE('',*,*,#5530,.T.);
#7326=ORIENTED_EDGE('',*,*,#5527,.T.);
#7327=ORIENTED_EDGE('',*,*,#5542,.F.);
#7328=ORIENTED_EDGE('',*,*,#5543,.T.);
#7329=ORIENTED_EDGE('',*,*,#5541,.T.);
#7330=ORIENTED_EDGE('',*,*,#5543,.F.);
#7331=ORIENTED_EDGE('',*,*,#5522,.T.);
#7332=ORIENTED_EDGE('',*,*,#5544,.T.);
#7333=ORIENTED_EDGE('',*,*,#5542,.T.);
#7334=ORIENTED_EDGE('',*,*,#5544,.F.);
#7335=ORIENTED_EDGE('',*,*,#5545,.F.);
#7336=ORIENTED_EDGE('',*,*,#5546,.T.);
#7337=ORIENTED_EDGE('',*,*,#5547,.F.);
#7338=ORIENTED_EDGE('',*,*,#5546,.F.);
#7339=ORIENTED_EDGE('',*,*,#5548,.F.);
#7340=ORIENTED_EDGE('',*,*,#5549,.T.);
#7341=ORIENTED_EDGE('',*,*,#5550,.F.);
#7342=ORIENTED_EDGE('',*,*,#5549,.F.);
#7343=ORIENTED_EDGE('',*,*,#5551,.F.);
#7344=ORIENTED_EDGE('',*,*,#5552,.F.);
#7345=ORIENTED_EDGE('',*,*,#5553,.F.);
#7346=ORIENTED_EDGE('',*,*,#5554,.T.);
#7347=ORIENTED_EDGE('',*,*,#5551,.T.);
#7348=ORIENTED_EDGE('',*,*,#5555,.F.);
#7349=ORIENTED_EDGE('',*,*,#5556,.F.);
#7350=ORIENTED_EDGE('',*,*,#5557,.F.);
#7351=ORIENTED_EDGE('',*,*,#5554,.F.);
#7352=ORIENTED_EDGE('',*,*,#5558,.T.);
#7353=ORIENTED_EDGE('',*,*,#5559,.F.);
#7354=ORIENTED_EDGE('',*,*,#5555,.T.);
#7355=ORIENTED_EDGE('',*,*,#5545,.T.);
#7356=ORIENTED_EDGE('',*,*,#5548,.T.);
#7357=ORIENTED_EDGE('',*,*,#5553,.T.);
#7358=ORIENTED_EDGE('',*,*,#5560,.F.);
#7359=ORIENTED_EDGE('',*,*,#5561,.F.);
#7360=ORIENTED_EDGE('',*,*,#5558,.F.);
#7361=ORIENTED_EDGE('',*,*,#5556,.T.);
#7362=ORIENTED_EDGE('',*,*,#5559,.T.);
#7363=ORIENTED_EDGE('',*,*,#5561,.T.);
#7364=ORIENTED_EDGE('',*,*,#5562,.F.);
#7365=ORIENTED_EDGE('',*,*,#5557,.T.);
#7366=ORIENTED_EDGE('',*,*,#5562,.T.);
#7367=ORIENTED_EDGE('',*,*,#5560,.T.);
#7368=ORIENTED_EDGE('',*,*,#5552,.T.);
#7369=ORIENTED_EDGE('',*,*,#5547,.T.);
#7370=ORIENTED_EDGE('',*,*,#5550,.T.);
#7371=ORIENTED_EDGE('',*,*,#5563,.F.);
#7372=ORIENTED_EDGE('',*,*,#5564,.T.);
#7373=ORIENTED_EDGE('',*,*,#5565,.T.);
#7374=ORIENTED_EDGE('',*,*,#5564,.F.);
#7375=ORIENTED_EDGE('',*,*,#5566,.F.);
#7376=ORIENTED_EDGE('',*,*,#5567,.T.);
#7377=ORIENTED_EDGE('',*,*,#5568,.T.);
#7378=ORIENTED_EDGE('',*,*,#5567,.F.);
#7379=ORIENTED_EDGE('',*,*,#5566,.T.);
#7380=ORIENTED_EDGE('',*,*,#5563,.T.);
#7381=ORIENTED_EDGE('',*,*,#5568,.F.);
#7382=ORIENTED_EDGE('',*,*,#5565,.F.);
#7383=ORIENTED_EDGE('',*,*,#5569,.F.);
#7384=ORIENTED_EDGE('',*,*,#5570,.T.);
#7385=ORIENTED_EDGE('',*,*,#5571,.T.);
#7386=ORIENTED_EDGE('',*,*,#5570,.F.);
#7387=ORIENTED_EDGE('',*,*,#5572,.F.);
#7388=ORIENTED_EDGE('',*,*,#5573,.T.);
#7389=ORIENTED_EDGE('',*,*,#5574,.T.);
#7390=ORIENTED_EDGE('',*,*,#5573,.F.);
#7391=ORIENTED_EDGE('',*,*,#5572,.T.);
#7392=ORIENTED_EDGE('',*,*,#5569,.T.);
#7393=ORIENTED_EDGE('',*,*,#5574,.F.);
#7394=ORIENTED_EDGE('',*,*,#5571,.F.);
#7395=ORIENTED_EDGE('',*,*,#5575,.F.);
#7396=ORIENTED_EDGE('',*,*,#5576,.T.);
#7397=ORIENTED_EDGE('',*,*,#5577,.F.);
#7398=ORIENTED_EDGE('',*,*,#5576,.F.);
#7399=ORIENTED_EDGE('',*,*,#5578,.F.);
#7400=ORIENTED_EDGE('',*,*,#5579,.T.);
#7401=ORIENTED_EDGE('',*,*,#5580,.F.);
#7402=ORIENTED_EDGE('',*,*,#5579,.F.);
#7403=ORIENTED_EDGE('',*,*,#5581,.F.);
#7404=ORIENTED_EDGE('',*,*,#5582,.F.);
#7405=ORIENTED_EDGE('',*,*,#5583,.F.);
#7406=ORIENTED_EDGE('',*,*,#5584,.T.);
#7407=ORIENTED_EDGE('',*,*,#5581,.T.);
#7408=ORIENTED_EDGE('',*,*,#5585,.F.);
#7409=ORIENTED_EDGE('',*,*,#5586,.F.);
#7410=ORIENTED_EDGE('',*,*,#5587,.F.);
#7411=ORIENTED_EDGE('',*,*,#5584,.F.);
#7412=ORIENTED_EDGE('',*,*,#5588,.T.);
#7413=ORIENTED_EDGE('',*,*,#5589,.F.);
#7414=ORIENTED_EDGE('',*,*,#5585,.T.);
#7415=ORIENTED_EDGE('',*,*,#5575,.T.);
#7416=ORIENTED_EDGE('',*,*,#5578,.T.);
#7417=ORIENTED_EDGE('',*,*,#5583,.T.);
#7418=ORIENTED_EDGE('',*,*,#5590,.F.);
#7419=ORIENTED_EDGE('',*,*,#5591,.F.);
#7420=ORIENTED_EDGE('',*,*,#5588,.F.);
#7421=ORIENTED_EDGE('',*,*,#5586,.T.);
#7422=ORIENTED_EDGE('',*,*,#5589,.T.);
#7423=ORIENTED_EDGE('',*,*,#5591,.T.);
#7424=ORIENTED_EDGE('',*,*,#5592,.F.);
#7425=ORIENTED_EDGE('',*,*,#5587,.T.);
#7426=ORIENTED_EDGE('',*,*,#5592,.T.);
#7427=ORIENTED_EDGE('',*,*,#5590,.T.);
#7428=ORIENTED_EDGE('',*,*,#5582,.T.);
#7429=ORIENTED_EDGE('',*,*,#5577,.T.);
#7430=ORIENTED_EDGE('',*,*,#5580,.T.);
#7431=ORIENTED_EDGE('',*,*,#5593,.F.);
#7432=ORIENTED_EDGE('',*,*,#5594,.T.);
#7433=ORIENTED_EDGE('',*,*,#5595,.T.);
#7434=ORIENTED_EDGE('',*,*,#5594,.F.);
#7435=ORIENTED_EDGE('',*,*,#5596,.F.);
#7436=ORIENTED_EDGE('',*,*,#5597,.T.);
#7437=ORIENTED_EDGE('',*,*,#5598,.T.);
#7438=ORIENTED_EDGE('',*,*,#5597,.F.);
#7439=ORIENTED_EDGE('',*,*,#5596,.T.);
#7440=ORIENTED_EDGE('',*,*,#5593,.T.);
#7441=ORIENTED_EDGE('',*,*,#5598,.F.);
#7442=ORIENTED_EDGE('',*,*,#5595,.F.);
#7443=ORIENTED_EDGE('',*,*,#5599,.F.);
#7444=ORIENTED_EDGE('',*,*,#5600,.T.);
#7445=ORIENTED_EDGE('',*,*,#5601,.T.);
#7446=ORIENTED_EDGE('',*,*,#5600,.F.);
#7447=ORIENTED_EDGE('',*,*,#5602,.F.);
#7448=ORIENTED_EDGE('',*,*,#5603,.T.);
#7449=ORIENTED_EDGE('',*,*,#5604,.T.);
#7450=ORIENTED_EDGE('',*,*,#5603,.F.);
#7451=ORIENTED_EDGE('',*,*,#5602,.T.);
#7452=ORIENTED_EDGE('',*,*,#5599,.T.);
#7453=ORIENTED_EDGE('',*,*,#5604,.F.);
#7454=ORIENTED_EDGE('',*,*,#5601,.F.);
#7455=ORIENTED_EDGE('',*,*,#5605,.F.);
#7456=ORIENTED_EDGE('',*,*,#5606,.T.);
#7457=ORIENTED_EDGE('',*,*,#5607,.F.);
#7458=ORIENTED_EDGE('',*,*,#5606,.F.);
#7459=ORIENTED_EDGE('',*,*,#5605,.T.);
#7460=ORIENTED_EDGE('',*,*,#5608,.F.);
#7461=ORIENTED_EDGE('',*,*,#5609,.T.);
#7462=ORIENTED_EDGE('',*,*,#5610,.F.);
#7463=ORIENTED_EDGE('',*,*,#5609,.F.);
#7464=ORIENTED_EDGE('',*,*,#5611,.F.);
#7465=ORIENTED_EDGE('',*,*,#5612,.T.);
#7466=ORIENTED_EDGE('',*,*,#5613,.F.);
#7467=ORIENTED_EDGE('',*,*,#5612,.F.);
#7468=ORIENTED_EDGE('',*,*,#5614,.F.);
#7469=ORIENTED_EDGE('',*,*,#5615,.T.);
#7470=ORIENTED_EDGE('',*,*,#5616,.F.);
#7471=ORIENTED_EDGE('',*,*,#5615,.F.);
#7472=ORIENTED_EDGE('',*,*,#5617,.F.);
#7473=ORIENTED_EDGE('',*,*,#5618,.T.);
#7474=ORIENTED_EDGE('',*,*,#5619,.F.);
#7475=ORIENTED_EDGE('',*,*,#5618,.F.);
#7476=ORIENTED_EDGE('',*,*,#5620,.F.);
#7477=ORIENTED_EDGE('',*,*,#5621,.T.);
#7478=ORIENTED_EDGE('',*,*,#5622,.F.);
#7479=ORIENTED_EDGE('',*,*,#5621,.F.);
#7480=ORIENTED_EDGE('',*,*,#5623,.T.);
#7481=ORIENTED_EDGE('',*,*,#5624,.T.);
#7482=ORIENTED_EDGE('',*,*,#5625,.F.);
#7483=ORIENTED_EDGE('',*,*,#5626,.F.);
#7484=ORIENTED_EDGE('',*,*,#5627,.T.);
#7485=ORIENTED_EDGE('',*,*,#5626,.T.);
#7486=ORIENTED_EDGE('',*,*,#5628,.F.);
#7487=ORIENTED_EDGE('',*,*,#5629,.F.);
#7488=ORIENTED_EDGE('',*,*,#5622,.T.);
#7489=ORIENTED_EDGE('',*,*,#5619,.T.);
#7490=ORIENTED_EDGE('',*,*,#5616,.T.);
#7491=ORIENTED_EDGE('',*,*,#5613,.T.);
#7492=ORIENTED_EDGE('',*,*,#5610,.T.);
#7493=ORIENTED_EDGE('',*,*,#5630,.T.);
#7494=ORIENTED_EDGE('',*,*,#5629,.T.);
#7495=ORIENTED_EDGE('',*,*,#5631,.F.);
#7496=ORIENTED_EDGE('',*,*,#5632,.F.);
#7497=ORIENTED_EDGE('',*,*,#5633,.T.);
#7498=ORIENTED_EDGE('',*,*,#5632,.T.);
#7499=ORIENTED_EDGE('',*,*,#5634,.F.);
#7500=ORIENTED_EDGE('',*,*,#5624,.F.);
#7501=ORIENTED_EDGE('',*,*,#5620,.T.);
#7502=ORIENTED_EDGE('',*,*,#5617,.T.);
#7503=ORIENTED_EDGE('',*,*,#5614,.T.);
#7504=ORIENTED_EDGE('',*,*,#5611,.T.);
#7505=ORIENTED_EDGE('',*,*,#5608,.T.);
#7506=ORIENTED_EDGE('',*,*,#5634,.T.);
#7507=ORIENTED_EDGE('',*,*,#5631,.T.);
#7508=ORIENTED_EDGE('',*,*,#5628,.T.);
#7509=ORIENTED_EDGE('',*,*,#5625,.T.);
#7510=ORIENTED_EDGE('',*,*,#5607,.T.);
#7511=ORIENTED_EDGE('',*,*,#5633,.F.);
#7512=ORIENTED_EDGE('',*,*,#5623,.F.);
#7513=ORIENTED_EDGE('',*,*,#5627,.F.);
#7514=ORIENTED_EDGE('',*,*,#5630,.F.);
#7515=ORIENTED_EDGE('',*,*,#5635,.F.);
#7516=ORIENTED_EDGE('',*,*,#5636,.T.);
#7517=ORIENTED_EDGE('',*,*,#5637,.F.);
#7518=ORIENTED_EDGE('',*,*,#5636,.F.);
#7519=ORIENTED_EDGE('',*,*,#5638,.F.);
#7520=ORIENTED_EDGE('',*,*,#5639,.T.);
#7521=ORIENTED_EDGE('',*,*,#5640,.F.);
#7522=ORIENTED_EDGE('',*,*,#5639,.F.);
#7523=ORIENTED_EDGE('',*,*,#5641,.F.);
#7524=ORIENTED_EDGE('',*,*,#5642,.T.);
#7525=ORIENTED_EDGE('',*,*,#5643,.F.);
#7526=ORIENTED_EDGE('',*,*,#5642,.F.);
#7527=ORIENTED_EDGE('',*,*,#5644,.F.);
#7528=ORIENTED_EDGE('',*,*,#5645,.T.);
#7529=ORIENTED_EDGE('',*,*,#5646,.F.);
#7530=ORIENTED_EDGE('',*,*,#5645,.F.);
#7531=ORIENTED_EDGE('',*,*,#5647,.F.);
#7532=ORIENTED_EDGE('',*,*,#5648,.T.);
#7533=ORIENTED_EDGE('',*,*,#5649,.F.);
#7534=ORIENTED_EDGE('',*,*,#5648,.F.);
#7535=ORIENTED_EDGE('',*,*,#5650,.T.);
#7536=ORIENTED_EDGE('',*,*,#5651,.T.);
#7537=ORIENTED_EDGE('',*,*,#5652,.F.);
#7538=ORIENTED_EDGE('',*,*,#5653,.F.);
#7539=ORIENTED_EDGE('',*,*,#5654,.T.);
#7540=ORIENTED_EDGE('',*,*,#5653,.T.);
#7541=ORIENTED_EDGE('',*,*,#5655,.F.);
#7542=ORIENTED_EDGE('',*,*,#5656,.F.);
#7543=ORIENTED_EDGE('',*,*,#5649,.T.);
#7544=ORIENTED_EDGE('',*,*,#5646,.T.);
#7545=ORIENTED_EDGE('',*,*,#5643,.T.);
#7546=ORIENTED_EDGE('',*,*,#5640,.T.);
#7547=ORIENTED_EDGE('',*,*,#5637,.T.);
#7548=ORIENTED_EDGE('',*,*,#5657,.T.);
#7549=ORIENTED_EDGE('',*,*,#5656,.T.);
#7550=ORIENTED_EDGE('',*,*,#5658,.F.);
#7551=ORIENTED_EDGE('',*,*,#5659,.F.);
#7552=ORIENTED_EDGE('',*,*,#5660,.T.);
#7553=ORIENTED_EDGE('',*,*,#5659,.T.);
#7554=ORIENTED_EDGE('',*,*,#5661,.F.);
#7555=ORIENTED_EDGE('',*,*,#5651,.F.);
#7556=ORIENTED_EDGE('',*,*,#5647,.T.);
#7557=ORIENTED_EDGE('',*,*,#5644,.T.);
#7558=ORIENTED_EDGE('',*,*,#5641,.T.);
#7559=ORIENTED_EDGE('',*,*,#5638,.T.);
#7560=ORIENTED_EDGE('',*,*,#5635,.T.);
#7561=ORIENTED_EDGE('',*,*,#5661,.T.);
#7562=ORIENTED_EDGE('',*,*,#5658,.T.);
#7563=ORIENTED_EDGE('',*,*,#5655,.T.);
#7564=ORIENTED_EDGE('',*,*,#5652,.T.);
#7565=ORIENTED_EDGE('',*,*,#5660,.F.);
#7566=ORIENTED_EDGE('',*,*,#5650,.F.);
#7567=ORIENTED_EDGE('',*,*,#5654,.F.);
#7568=ORIENTED_EDGE('',*,*,#5657,.F.);
#7569=ORIENTED_EDGE('',*,*,#5662,.F.);
#7570=ORIENTED_EDGE('',*,*,#5663,.T.);
#7571=ORIENTED_EDGE('',*,*,#5664,.F.);
#7572=ORIENTED_EDGE('',*,*,#5663,.F.);
#7573=ORIENTED_EDGE('',*,*,#5665,.F.);
#7574=ORIENTED_EDGE('',*,*,#5666,.T.);
#7575=ORIENTED_EDGE('',*,*,#5667,.F.);
#7576=ORIENTED_EDGE('',*,*,#5666,.F.);
#7577=ORIENTED_EDGE('',*,*,#5668,.F.);
#7578=ORIENTED_EDGE('',*,*,#5669,.T.);
#7579=ORIENTED_EDGE('',*,*,#5670,.F.);
#7580=ORIENTED_EDGE('',*,*,#5669,.F.);
#7581=ORIENTED_EDGE('',*,*,#5671,.F.);
#7582=ORIENTED_EDGE('',*,*,#5672,.T.);
#7583=ORIENTED_EDGE('',*,*,#5673,.F.);
#7584=ORIENTED_EDGE('',*,*,#5672,.F.);
#7585=ORIENTED_EDGE('',*,*,#5674,.F.);
#7586=ORIENTED_EDGE('',*,*,#5675,.T.);
#7587=ORIENTED_EDGE('',*,*,#5676,.F.);
#7588=ORIENTED_EDGE('',*,*,#5675,.F.);
#7589=ORIENTED_EDGE('',*,*,#5677,.T.);
#7590=ORIENTED_EDGE('',*,*,#5678,.T.);
#7591=ORIENTED_EDGE('',*,*,#5679,.F.);
#7592=ORIENTED_EDGE('',*,*,#5680,.F.);
#7593=ORIENTED_EDGE('',*,*,#5681,.T.);
#7594=ORIENTED_EDGE('',*,*,#5680,.T.);
#7595=ORIENTED_EDGE('',*,*,#5682,.F.);
#7596=ORIENTED_EDGE('',*,*,#5683,.F.);
#7597=ORIENTED_EDGE('',*,*,#5676,.T.);
#7598=ORIENTED_EDGE('',*,*,#5673,.T.);
#7599=ORIENTED_EDGE('',*,*,#5670,.T.);
#7600=ORIENTED_EDGE('',*,*,#5667,.T.);
#7601=ORIENTED_EDGE('',*,*,#5664,.T.);
#7602=ORIENTED_EDGE('',*,*,#5684,.T.);
#7603=ORIENTED_EDGE('',*,*,#5683,.T.);
#7604=ORIENTED_EDGE('',*,*,#5685,.F.);
#7605=ORIENTED_EDGE('',*,*,#5686,.F.);
#7606=ORIENTED_EDGE('',*,*,#5687,.T.);
#7607=ORIENTED_EDGE('',*,*,#5686,.T.);
#7608=ORIENTED_EDGE('',*,*,#5688,.F.);
#7609=ORIENTED_EDGE('',*,*,#5678,.F.);
#7610=ORIENTED_EDGE('',*,*,#5674,.T.);
#7611=ORIENTED_EDGE('',*,*,#5671,.T.);
#7612=ORIENTED_EDGE('',*,*,#5668,.T.);
#7613=ORIENTED_EDGE('',*,*,#5665,.T.);
#7614=ORIENTED_EDGE('',*,*,#5662,.T.);
#7615=ORIENTED_EDGE('',*,*,#5688,.T.);
#7616=ORIENTED_EDGE('',*,*,#5685,.T.);
#7617=ORIENTED_EDGE('',*,*,#5682,.T.);
#7618=ORIENTED_EDGE('',*,*,#5679,.T.);
#7619=ORIENTED_EDGE('',*,*,#5687,.F.);
#7620=ORIENTED_EDGE('',*,*,#5677,.F.);
#7621=ORIENTED_EDGE('',*,*,#5681,.F.);
#7622=ORIENTED_EDGE('',*,*,#5684,.F.);
#7623=ORIENTED_EDGE('',*,*,#5689,.F.);
#7624=ORIENTED_EDGE('',*,*,#5690,.T.);
#7625=ORIENTED_EDGE('',*,*,#5691,.F.);
#7626=ORIENTED_EDGE('',*,*,#5690,.F.);
#7627=ORIENTED_EDGE('',*,*,#5689,.T.);
#7628=ORIENTED_EDGE('',*,*,#5692,.T.);
#7629=ORIENTED_EDGE('',*,*,#5693,.F.);
#7630=ORIENTED_EDGE('',*,*,#5694,.F.);
#7631=ORIENTED_EDGE('',*,*,#5695,.F.);
#7632=ORIENTED_EDGE('',*,*,#5692,.F.);
#7633=ORIENTED_EDGE('',*,*,#5696,.T.);
#7634=ORIENTED_EDGE('',*,*,#5694,.T.);
#7635=ORIENTED_EDGE('',*,*,#5696,.F.);
#7636=ORIENTED_EDGE('',*,*,#5695,.T.);
#7637=ORIENTED_EDGE('',*,*,#5697,.T.);
#7638=ORIENTED_EDGE('',*,*,#5698,.T.);
#7639=ORIENTED_EDGE('',*,*,#5697,.F.);
#7640=ORIENTED_EDGE('',*,*,#5699,.F.);
#7641=ORIENTED_EDGE('',*,*,#5700,.T.);
#7642=ORIENTED_EDGE('',*,*,#5693,.T.);
#7643=ORIENTED_EDGE('',*,*,#5700,.F.);
#7644=ORIENTED_EDGE('',*,*,#5699,.T.);
#7645=ORIENTED_EDGE('',*,*,#5691,.T.);
#7646=ORIENTED_EDGE('',*,*,#5698,.F.);
#7647=ORIENTED_EDGE('',*,*,#5701,.F.);
#7648=ORIENTED_EDGE('',*,*,#5702,.T.);
#7649=ORIENTED_EDGE('',*,*,#5703,.T.);
#7650=ORIENTED_EDGE('',*,*,#5702,.F.);
#7651=ORIENTED_EDGE('',*,*,#5704,.F.);
#7652=ORIENTED_EDGE('',*,*,#5705,.T.);
#7653=ORIENTED_EDGE('',*,*,#5706,.T.);
#7654=ORIENTED_EDGE('',*,*,#5705,.F.);
#7655=ORIENTED_EDGE('',*,*,#5704,.T.);
#7656=ORIENTED_EDGE('',*,*,#5701,.T.);
#7657=ORIENTED_EDGE('',*,*,#5706,.F.);
#7658=ORIENTED_EDGE('',*,*,#5703,.F.);
#7659=ORIENTED_EDGE('',*,*,#5707,.F.);
#7660=ORIENTED_EDGE('',*,*,#5708,.T.);
#7661=ORIENTED_EDGE('',*,*,#5709,.T.);
#7662=ORIENTED_EDGE('',*,*,#5708,.F.);
#7663=ORIENTED_EDGE('',*,*,#5710,.F.);
#7664=ORIENTED_EDGE('',*,*,#5711,.T.);
#7665=ORIENTED_EDGE('',*,*,#5712,.T.);
#7666=ORIENTED_EDGE('',*,*,#5711,.F.);
#7667=ORIENTED_EDGE('',*,*,#5710,.T.);
#7668=ORIENTED_EDGE('',*,*,#5707,.T.);
#7669=ORIENTED_EDGE('',*,*,#5712,.F.);
#7670=ORIENTED_EDGE('',*,*,#5709,.F.);
#7671=ORIENTED_EDGE('',*,*,#5713,.F.);
#7672=ORIENTED_EDGE('',*,*,#5714,.T.);
#7673=ORIENTED_EDGE('',*,*,#5715,.T.);
#7674=ORIENTED_EDGE('',*,*,#5714,.F.);
#7675=ORIENTED_EDGE('',*,*,#5716,.F.);
#7676=ORIENTED_EDGE('',*,*,#5717,.T.);
#7677=ORIENTED_EDGE('',*,*,#5718,.T.);
#7678=ORIENTED_EDGE('',*,*,#5717,.F.);
#7679=ORIENTED_EDGE('',*,*,#5716,.T.);
#7680=ORIENTED_EDGE('',*,*,#5713,.T.);
#7681=ORIENTED_EDGE('',*,*,#5718,.F.);
#7682=ORIENTED_EDGE('',*,*,#5715,.F.);
#7683=ORIENTED_EDGE('',*,*,#5719,.F.);
#7684=ORIENTED_EDGE('',*,*,#5720,.T.);
#7685=ORIENTED_EDGE('',*,*,#5721,.F.);
#7686=ORIENTED_EDGE('',*,*,#5720,.F.);
#7687=ORIENTED_EDGE('',*,*,#5719,.T.);
#7688=ORIENTED_EDGE('',*,*,#5722,.F.);
#7689=ORIENTED_EDGE('',*,*,#5723,.T.);
#7690=ORIENTED_EDGE('',*,*,#5724,.F.);
#7691=ORIENTED_EDGE('',*,*,#5723,.F.);
#7692=ORIENTED_EDGE('',*,*,#5725,.F.);
#7693=ORIENTED_EDGE('',*,*,#5726,.T.);
#7694=ORIENTED_EDGE('',*,*,#5727,.F.);
#7695=ORIENTED_EDGE('',*,*,#5726,.F.);
#7696=ORIENTED_EDGE('',*,*,#5728,.F.);
#7697=ORIENTED_EDGE('',*,*,#5729,.T.);
#7698=ORIENTED_EDGE('',*,*,#5730,.F.);
#7699=ORIENTED_EDGE('',*,*,#5729,.F.);
#7700=ORIENTED_EDGE('',*,*,#5731,.F.);
#7701=ORIENTED_EDGE('',*,*,#5732,.T.);
#7702=ORIENTED_EDGE('',*,*,#5733,.F.);
#7703=ORIENTED_EDGE('',*,*,#5732,.F.);
#7704=ORIENTED_EDGE('',*,*,#5734,.F.);
#7705=ORIENTED_EDGE('',*,*,#5735,.T.);
#7706=ORIENTED_EDGE('',*,*,#5736,.F.);
#7707=ORIENTED_EDGE('',*,*,#5735,.F.);
#7708=ORIENTED_EDGE('',*,*,#5737,.T.);
#7709=ORIENTED_EDGE('',*,*,#5738,.T.);
#7710=ORIENTED_EDGE('',*,*,#5739,.F.);
#7711=ORIENTED_EDGE('',*,*,#5740,.F.);
#7712=ORIENTED_EDGE('',*,*,#5736,.T.);
#7713=ORIENTED_EDGE('',*,*,#5733,.T.);
#7714=ORIENTED_EDGE('',*,*,#5730,.T.);
#7715=ORIENTED_EDGE('',*,*,#5727,.T.);
#7716=ORIENTED_EDGE('',*,*,#5724,.T.);
#7717=ORIENTED_EDGE('',*,*,#5741,.T.);
#7718=ORIENTED_EDGE('',*,*,#5740,.T.);
#7719=ORIENTED_EDGE('',*,*,#5742,.F.);
#7720=ORIENTED_EDGE('',*,*,#5743,.F.);
#7721=ORIENTED_EDGE('',*,*,#5744,.T.);
#7722=ORIENTED_EDGE('',*,*,#5743,.T.);
#7723=ORIENTED_EDGE('',*,*,#5745,.F.);
#7724=ORIENTED_EDGE('',*,*,#5746,.F.);
#7725=ORIENTED_EDGE('',*,*,#5734,.T.);
#7726=ORIENTED_EDGE('',*,*,#5731,.T.);
#7727=ORIENTED_EDGE('',*,*,#5728,.T.);
#7728=ORIENTED_EDGE('',*,*,#5725,.T.);
#7729=ORIENTED_EDGE('',*,*,#5722,.T.);
#7730=ORIENTED_EDGE('',*,*,#5747,.T.);
#7731=ORIENTED_EDGE('',*,*,#5746,.T.);
#7732=ORIENTED_EDGE('',*,*,#5748,.F.);
#7733=ORIENTED_EDGE('',*,*,#5738,.F.);
#7734=ORIENTED_EDGE('',*,*,#5748,.T.);
#7735=ORIENTED_EDGE('',*,*,#5745,.T.);
#7736=ORIENTED_EDGE('',*,*,#5742,.T.);
#7737=ORIENTED_EDGE('',*,*,#5739,.T.);
#7738=ORIENTED_EDGE('',*,*,#5721,.T.);
#7739=ORIENTED_EDGE('',*,*,#5747,.F.);
#7740=ORIENTED_EDGE('',*,*,#5737,.F.);
#7741=ORIENTED_EDGE('',*,*,#5741,.F.);
#7742=ORIENTED_EDGE('',*,*,#5744,.F.);
#7743=ORIENTED_EDGE('',*,*,#5749,.F.);
#7744=ORIENTED_EDGE('',*,*,#5750,.T.);
#7745=ORIENTED_EDGE('',*,*,#5751,.F.);
#7746=ORIENTED_EDGE('',*,*,#5750,.F.);
#7747=ORIENTED_EDGE('',*,*,#5752,.F.);
#7748=ORIENTED_EDGE('',*,*,#5753,.T.);
#7749=ORIENTED_EDGE('',*,*,#5754,.F.);
#7750=ORIENTED_EDGE('',*,*,#5753,.F.);
#7751=ORIENTED_EDGE('',*,*,#5755,.F.);
#7752=ORIENTED_EDGE('',*,*,#5756,.T.);
#7753=ORIENTED_EDGE('',*,*,#5757,.F.);
#7754=ORIENTED_EDGE('',*,*,#5756,.F.);
#7755=ORIENTED_EDGE('',*,*,#5758,.F.);
#7756=ORIENTED_EDGE('',*,*,#5759,.T.);
#7757=ORIENTED_EDGE('',*,*,#5760,.F.);
#7758=ORIENTED_EDGE('',*,*,#5759,.F.);
#7759=ORIENTED_EDGE('',*,*,#5761,.F.);
#7760=ORIENTED_EDGE('',*,*,#5762,.T.);
#7761=ORIENTED_EDGE('',*,*,#5763,.F.);
#7762=ORIENTED_EDGE('',*,*,#5762,.F.);
#7763=ORIENTED_EDGE('',*,*,#5764,.T.);
#7764=ORIENTED_EDGE('',*,*,#5765,.T.);
#7765=ORIENTED_EDGE('',*,*,#5766,.F.);
#7766=ORIENTED_EDGE('',*,*,#5767,.F.);
#7767=ORIENTED_EDGE('',*,*,#5763,.T.);
#7768=ORIENTED_EDGE('',*,*,#5760,.T.);
#7769=ORIENTED_EDGE('',*,*,#5757,.T.);
#7770=ORIENTED_EDGE('',*,*,#5754,.T.);
#7771=ORIENTED_EDGE('',*,*,#5751,.T.);
#7772=ORIENTED_EDGE('',*,*,#5768,.T.);
#7773=ORIENTED_EDGE('',*,*,#5767,.T.);
#7774=ORIENTED_EDGE('',*,*,#5769,.F.);
#7775=ORIENTED_EDGE('',*,*,#5770,.F.);
#7776=ORIENTED_EDGE('',*,*,#5771,.T.);
#7777=ORIENTED_EDGE('',*,*,#5770,.T.);
#7778=ORIENTED_EDGE('',*,*,#5772,.F.);
#7779=ORIENTED_EDGE('',*,*,#5773,.F.);
#7780=ORIENTED_EDGE('',*,*,#5761,.T.);
#7781=ORIENTED_EDGE('',*,*,#5758,.T.);
#7782=ORIENTED_EDGE('',*,*,#5755,.T.);
#7783=ORIENTED_EDGE('',*,*,#5752,.T.);
#7784=ORIENTED_EDGE('',*,*,#5749,.T.);
#7785=ORIENTED_EDGE('',*,*,#5774,.T.);
#7786=ORIENTED_EDGE('',*,*,#5773,.T.);
#7787=ORIENTED_EDGE('',*,*,#5775,.F.);
#7788=ORIENTED_EDGE('',*,*,#5765,.F.);
#7789=ORIENTED_EDGE('',*,*,#5775,.T.);
#7790=ORIENTED_EDGE('',*,*,#5772,.T.);
#7791=ORIENTED_EDGE('',*,*,#5769,.T.);
#7792=ORIENTED_EDGE('',*,*,#5766,.T.);
#7793=ORIENTED_EDGE('',*,*,#5774,.F.);
#7794=ORIENTED_EDGE('',*,*,#5764,.F.);
#7795=ORIENTED_EDGE('',*,*,#5768,.F.);
#7796=ORIENTED_EDGE('',*,*,#5771,.F.);
#7797=ORIENTED_EDGE('',*,*,#5776,.F.);
#7798=ORIENTED_EDGE('',*,*,#5777,.T.);
#7799=ORIENTED_EDGE('',*,*,#5778,.F.);
#7800=ORIENTED_EDGE('',*,*,#5777,.F.);
#7801=ORIENTED_EDGE('',*,*,#5779,.F.);
#7802=ORIENTED_EDGE('',*,*,#5780,.T.);
#7803=ORIENTED_EDGE('',*,*,#5781,.F.);
#7804=ORIENTED_EDGE('',*,*,#5780,.F.);
#7805=ORIENTED_EDGE('',*,*,#5782,.F.);
#7806=ORIENTED_EDGE('',*,*,#5783,.T.);
#7807=ORIENTED_EDGE('',*,*,#5784,.F.);
#7808=ORIENTED_EDGE('',*,*,#5783,.F.);
#7809=ORIENTED_EDGE('',*,*,#5785,.F.);
#7810=ORIENTED_EDGE('',*,*,#5786,.T.);
#7811=ORIENTED_EDGE('',*,*,#5787,.F.);
#7812=ORIENTED_EDGE('',*,*,#5786,.F.);
#7813=ORIENTED_EDGE('',*,*,#5788,.F.);
#7814=ORIENTED_EDGE('',*,*,#5789,.T.);
#7815=ORIENTED_EDGE('',*,*,#5790,.F.);
#7816=ORIENTED_EDGE('',*,*,#5789,.F.);
#7817=ORIENTED_EDGE('',*,*,#5791,.T.);
#7818=ORIENTED_EDGE('',*,*,#5792,.T.);
#7819=ORIENTED_EDGE('',*,*,#5793,.F.);
#7820=ORIENTED_EDGE('',*,*,#5794,.F.);
#7821=ORIENTED_EDGE('',*,*,#5790,.T.);
#7822=ORIENTED_EDGE('',*,*,#5787,.T.);
#7823=ORIENTED_EDGE('',*,*,#5784,.T.);
#7824=ORIENTED_EDGE('',*,*,#5781,.T.);
#7825=ORIENTED_EDGE('',*,*,#5778,.T.);
#7826=ORIENTED_EDGE('',*,*,#5795,.T.);
#7827=ORIENTED_EDGE('',*,*,#5794,.T.);
#7828=ORIENTED_EDGE('',*,*,#5796,.F.);
#7829=ORIENTED_EDGE('',*,*,#5797,.F.);
#7830=ORIENTED_EDGE('',*,*,#5798,.T.);
#7831=ORIENTED_EDGE('',*,*,#5797,.T.);
#7832=ORIENTED_EDGE('',*,*,#5799,.F.);
#7833=ORIENTED_EDGE('',*,*,#5800,.F.);
#7834=ORIENTED_EDGE('',*,*,#5788,.T.);
#7835=ORIENTED_EDGE('',*,*,#5785,.T.);
#7836=ORIENTED_EDGE('',*,*,#5782,.T.);
#7837=ORIENTED_EDGE('',*,*,#5779,.T.);
#7838=ORIENTED_EDGE('',*,*,#5776,.T.);
#7839=ORIENTED_EDGE('',*,*,#5801,.T.);
#7840=ORIENTED_EDGE('',*,*,#5800,.T.);
#7841=ORIENTED_EDGE('',*,*,#5802,.F.);
#7842=ORIENTED_EDGE('',*,*,#5792,.F.);
#7843=ORIENTED_EDGE('',*,*,#5802,.T.);
#7844=ORIENTED_EDGE('',*,*,#5799,.T.);
#7845=ORIENTED_EDGE('',*,*,#5796,.T.);
#7846=ORIENTED_EDGE('',*,*,#5793,.T.);
#7847=ORIENTED_EDGE('',*,*,#5801,.F.);
#7848=ORIENTED_EDGE('',*,*,#5791,.F.);
#7849=ORIENTED_EDGE('',*,*,#5795,.F.);
#7850=ORIENTED_EDGE('',*,*,#5798,.F.);
#7851=ORIENTED_EDGE('',*,*,#5803,.F.);
#7852=ORIENTED_EDGE('',*,*,#5804,.T.);
#7853=ORIENTED_EDGE('',*,*,#5805,.F.);
#7854=ORIENTED_EDGE('',*,*,#5804,.F.);
#7855=ORIENTED_EDGE('',*,*,#5803,.T.);
#7856=ORIENTED_EDGE('',*,*,#5806,.T.);
#7857=ORIENTED_EDGE('',*,*,#5807,.F.);
#7858=ORIENTED_EDGE('',*,*,#5808,.F.);
#7859=ORIENTED_EDGE('',*,*,#5809,.F.);
#7860=ORIENTED_EDGE('',*,*,#5806,.F.);
#7861=ORIENTED_EDGE('',*,*,#5810,.T.);
#7862=ORIENTED_EDGE('',*,*,#5808,.T.);
#7863=ORIENTED_EDGE('',*,*,#5810,.F.);
#7864=ORIENTED_EDGE('',*,*,#5809,.T.);
#7865=ORIENTED_EDGE('',*,*,#5811,.T.);
#7866=ORIENTED_EDGE('',*,*,#5812,.T.);
#7867=ORIENTED_EDGE('',*,*,#5811,.F.);
#7868=ORIENTED_EDGE('',*,*,#5813,.F.);
#7869=ORIENTED_EDGE('',*,*,#5814,.T.);
#7870=ORIENTED_EDGE('',*,*,#5807,.T.);
#7871=ORIENTED_EDGE('',*,*,#5814,.F.);
#7872=ORIENTED_EDGE('',*,*,#5813,.T.);
#7873=ORIENTED_EDGE('',*,*,#5805,.T.);
#7874=ORIENTED_EDGE('',*,*,#5812,.F.);
#7875=ORIENTED_EDGE('',*,*,#5815,.F.);
#7876=ORIENTED_EDGE('',*,*,#5816,.T.);
#7877=ORIENTED_EDGE('',*,*,#5817,.T.);
#7878=ORIENTED_EDGE('',*,*,#5816,.F.);
#7879=ORIENTED_EDGE('',*,*,#5818,.F.);
#7880=ORIENTED_EDGE('',*,*,#5819,.T.);
#7881=ORIENTED_EDGE('',*,*,#5820,.T.);
#7882=ORIENTED_EDGE('',*,*,#5819,.F.);
#7883=ORIENTED_EDGE('',*,*,#5818,.T.);
#7884=ORIENTED_EDGE('',*,*,#5815,.T.);
#7885=ORIENTED_EDGE('',*,*,#5820,.F.);
#7886=ORIENTED_EDGE('',*,*,#5817,.F.);
#7887=ORIENTED_EDGE('',*,*,#5821,.F.);
#7888=ORIENTED_EDGE('',*,*,#5822,.T.);
#7889=ORIENTED_EDGE('',*,*,#5823,.T.);
#7890=ORIENTED_EDGE('',*,*,#5822,.F.);
#7891=ORIENTED_EDGE('',*,*,#5824,.F.);
#7892=ORIENTED_EDGE('',*,*,#5825,.T.);
#7893=ORIENTED_EDGE('',*,*,#5826,.T.);
#7894=ORIENTED_EDGE('',*,*,#5825,.F.);
#7895=ORIENTED_EDGE('',*,*,#5824,.T.);
#7896=ORIENTED_EDGE('',*,*,#5821,.T.);
#7897=ORIENTED_EDGE('',*,*,#5826,.F.);
#7898=ORIENTED_EDGE('',*,*,#5823,.F.);
#7899=ORIENTED_EDGE('',*,*,#5827,.F.);
#7900=ORIENTED_EDGE('',*,*,#5828,.T.);
#7901=ORIENTED_EDGE('',*,*,#5829,.T.);
#7902=ORIENTED_EDGE('',*,*,#5828,.F.);
#7903=ORIENTED_EDGE('',*,*,#5830,.F.);
#7904=ORIENTED_EDGE('',*,*,#5831,.T.);
#7905=ORIENTED_EDGE('',*,*,#5832,.T.);
#7906=ORIENTED_EDGE('',*,*,#5831,.F.);
#7907=ORIENTED_EDGE('',*,*,#5830,.T.);
#7908=ORIENTED_EDGE('',*,*,#5827,.T.);
#7909=ORIENTED_EDGE('',*,*,#5832,.F.);
#7910=ORIENTED_EDGE('',*,*,#5829,.F.);
#7911=ORIENTED_EDGE('',*,*,#5833,.F.);
#7912=ORIENTED_EDGE('',*,*,#5834,.F.);
#7913=ORIENTED_EDGE('',*,*,#5835,.F.);
#7914=ORIENTED_EDGE('',*,*,#5836,.F.);
#7915=ORIENTED_EDGE('',*,*,#5837,.F.);
#7916=ORIENTED_EDGE('',*,*,#5836,.T.);
#7917=ORIENTED_EDGE('',*,*,#5838,.F.);
#7918=ORIENTED_EDGE('',*,*,#5839,.T.);
#7919=ORIENTED_EDGE('',*,*,#5840,.F.);
#7920=ORIENTED_EDGE('',*,*,#5839,.F.);
#7921=ORIENTED_EDGE('',*,*,#5841,.F.);
#7922=ORIENTED_EDGE('',*,*,#5842,.F.);
#7923=ORIENTED_EDGE('',*,*,#5843,.F.);
#7924=ORIENTED_EDGE('',*,*,#5842,.T.);
#7925=ORIENTED_EDGE('',*,*,#5844,.T.);
#7926=ORIENTED_EDGE('',*,*,#5834,.T.);
#7927=ORIENTED_EDGE('',*,*,#5844,.F.);
#7928=ORIENTED_EDGE('',*,*,#5841,.T.);
#7929=ORIENTED_EDGE('',*,*,#5838,.T.);
#7930=ORIENTED_EDGE('',*,*,#5835,.T.);
#7931=ORIENTED_EDGE('',*,*,#5845,.F.);
#7932=ORIENTED_EDGE('',*,*,#5846,.T.);
#7933=ORIENTED_EDGE('',*,*,#5847,.F.);
#7934=ORIENTED_EDGE('',*,*,#5848,.T.);
#7935=ORIENTED_EDGE('',*,*,#5845,.T.);
#7936=ORIENTED_EDGE('',*,*,#5848,.F.);
#7937=ORIENTED_EDGE('',*,*,#5847,.T.);
#7938=ORIENTED_EDGE('',*,*,#5849,.F.);
#7939=ORIENTED_EDGE('',*,*,#5850,.F.);
#7940=ORIENTED_EDGE('',*,*,#5851,.T.);
#7941=ORIENTED_EDGE('',*,*,#5849,.T.);
#7942=ORIENTED_EDGE('',*,*,#5851,.F.);
#7943=ORIENTED_EDGE('',*,*,#5852,.F.);
#7944=ORIENTED_EDGE('',*,*,#5850,.T.);
#7945=ORIENTED_EDGE('',*,*,#5853,.F.);
#7946=ORIENTED_EDGE('',*,*,#5854,.T.);
#7947=ORIENTED_EDGE('',*,*,#5852,.T.);
#7948=ORIENTED_EDGE('',*,*,#5854,.F.);
#7949=ORIENTED_EDGE('',*,*,#5853,.T.);
#7950=ORIENTED_EDGE('',*,*,#5855,.F.);
#7951=ORIENTED_EDGE('',*,*,#5856,.F.);
#7952=ORIENTED_EDGE('',*,*,#5857,.T.);
#7953=ORIENTED_EDGE('',*,*,#5855,.T.);
#7954=ORIENTED_EDGE('',*,*,#5857,.F.);
#7955=ORIENTED_EDGE('',*,*,#5858,.F.);
#7956=ORIENTED_EDGE('',*,*,#5856,.T.);
#7957=ORIENTED_EDGE('',*,*,#5859,.F.);
#7958=ORIENTED_EDGE('',*,*,#5860,.T.);
#7959=ORIENTED_EDGE('',*,*,#5858,.T.);
#7960=ORIENTED_EDGE('',*,*,#5860,.F.);
#7961=ORIENTED_EDGE('',*,*,#5859,.T.);
#7962=ORIENTED_EDGE('',*,*,#5861,.F.);
#7963=ORIENTED_EDGE('',*,*,#5861,.T.);
#7964=ORIENTED_EDGE('',*,*,#5862,.T.);
#7965=ORIENTED_EDGE('',*,*,#5846,.F.);
#7966=ORIENTED_EDGE('',*,*,#5862,.F.);
#7967=ORIENTED_EDGE('',*,*,#5840,.T.);
#7968=ORIENTED_EDGE('',*,*,#5843,.T.);
#7969=ORIENTED_EDGE('',*,*,#5833,.T.);
#7970=ORIENTED_EDGE('',*,*,#5837,.T.);
#7971=ORIENTED_EDGE('',*,*,#5863,.F.);
#7972=ORIENTED_EDGE('',*,*,#5864,.F.);
#7973=ORIENTED_EDGE('',*,*,#5865,.F.);
#7974=ORIENTED_EDGE('',*,*,#5866,.F.);
#7975=ORIENTED_EDGE('',*,*,#5867,.F.);
#7976=ORIENTED_EDGE('',*,*,#5866,.T.);
#7977=ORIENTED_EDGE('',*,*,#5868,.F.);
#7978=ORIENTED_EDGE('',*,*,#5869,.T.);
#7979=ORIENTED_EDGE('',*,*,#5870,.F.);
#7980=ORIENTED_EDGE('',*,*,#5869,.F.);
#7981=ORIENTED_EDGE('',*,*,#5871,.F.);
#7982=ORIENTED_EDGE('',*,*,#5872,.F.);
#7983=ORIENTED_EDGE('',*,*,#5873,.F.);
#7984=ORIENTED_EDGE('',*,*,#5872,.T.);
#7985=ORIENTED_EDGE('',*,*,#5874,.F.);
#7986=ORIENTED_EDGE('',*,*,#5864,.T.);
#7987=ORIENTED_EDGE('',*,*,#5875,.F.);
#7988=ORIENTED_EDGE('',*,*,#5876,.T.);
#7989=ORIENTED_EDGE('',*,*,#5877,.F.);
#7990=ORIENTED_EDGE('',*,*,#5878,.T.);
#7991=ORIENTED_EDGE('',*,*,#5875,.T.);
#7992=ORIENTED_EDGE('',*,*,#5878,.F.);
#7993=ORIENTED_EDGE('',*,*,#5870,.T.);
#7994=ORIENTED_EDGE('',*,*,#5873,.T.);
#7995=ORIENTED_EDGE('',*,*,#5863,.T.);
#7996=ORIENTED_EDGE('',*,*,#5867,.T.);
#7997=ORIENTED_EDGE('',*,*,#5877,.T.);
#7998=ORIENTED_EDGE('',*,*,#5879,.F.);
#7999=ORIENTED_EDGE('',*,*,#5879,.T.);
#8000=ORIENTED_EDGE('',*,*,#5880,.T.);
#8001=ORIENTED_EDGE('',*,*,#5876,.F.);
#8002=ORIENTED_EDGE('',*,*,#5880,.F.);
#8003=ORIENTED_EDGE('',*,*,#5871,.T.);
#8004=ORIENTED_EDGE('',*,*,#5868,.T.);
#8005=ORIENTED_EDGE('',*,*,#5865,.T.);
#8006=ORIENTED_EDGE('',*,*,#5874,.T.);
#8007=ORIENTED_EDGE('',*,*,#5881,.T.);
#8008=ORIENTED_EDGE('',*,*,#5882,.T.);
#8009=ORIENTED_EDGE('',*,*,#5883,.T.);
#8010=ORIENTED_EDGE('',*,*,#5884,.F.);
#8011=ORIENTED_EDGE('',*,*,#5885,.T.);
#8012=ORIENTED_EDGE('',*,*,#5886,.T.);
#8013=ORIENTED_EDGE('',*,*,#5887,.T.);
#8014=ORIENTED_EDGE('',*,*,#5882,.F.);
#8015=ORIENTED_EDGE('',*,*,#5888,.T.);
#8016=ORIENTED_EDGE('',*,*,#5889,.T.);
#8017=ORIENTED_EDGE('',*,*,#5890,.T.);
#8018=ORIENTED_EDGE('',*,*,#5886,.F.);
#8019=ORIENTED_EDGE('',*,*,#5891,.T.);
#8020=ORIENTED_EDGE('',*,*,#5892,.T.);
#8021=ORIENTED_EDGE('',*,*,#5893,.T.);
#8022=ORIENTED_EDGE('',*,*,#5889,.F.);
#8023=ORIENTED_EDGE('',*,*,#5894,.T.);
#8024=ORIENTED_EDGE('',*,*,#5895,.T.);
#8025=ORIENTED_EDGE('',*,*,#5896,.T.);
#8026=ORIENTED_EDGE('',*,*,#5892,.F.);
#8027=ORIENTED_EDGE('',*,*,#5897,.T.);
#8028=ORIENTED_EDGE('',*,*,#5884,.T.);
#8029=ORIENTED_EDGE('',*,*,#5898,.T.);
#8030=ORIENTED_EDGE('',*,*,#5895,.F.);
#8031=ORIENTED_EDGE('',*,*,#5897,.F.);
#8032=ORIENTED_EDGE('',*,*,#5894,.F.);
#8033=ORIENTED_EDGE('',*,*,#5891,.F.);
#8034=ORIENTED_EDGE('',*,*,#5888,.F.);
#8035=ORIENTED_EDGE('',*,*,#5885,.F.);
#8036=ORIENTED_EDGE('',*,*,#5881,.F.);
#8037=ORIENTED_EDGE('',*,*,#5898,.F.);
#8038=ORIENTED_EDGE('',*,*,#5883,.F.);
#8039=ORIENTED_EDGE('',*,*,#5887,.F.);
#8040=ORIENTED_EDGE('',*,*,#5890,.F.);
#8041=ORIENTED_EDGE('',*,*,#5893,.F.);
#8042=ORIENTED_EDGE('',*,*,#5896,.F.);
#8043=ORIENTED_EDGE('',*,*,#5899,.F.);
#8044=ORIENTED_EDGE('',*,*,#5900,.F.);
#8045=ORIENTED_EDGE('',*,*,#5901,.F.);
#8046=ORIENTED_EDGE('',*,*,#5902,.T.);
#8047=ORIENTED_EDGE('',*,*,#5900,.T.);
#8048=ORIENTED_EDGE('',*,*,#5902,.F.);
#8049=ORIENTED_EDGE('',*,*,#5903,.F.);
#8050=ORIENTED_EDGE('',*,*,#5904,.T.);
#8051=ORIENTED_EDGE('',*,*,#5901,.T.);
#8052=ORIENTED_EDGE('',*,*,#5904,.F.);
#8053=ORIENTED_EDGE('',*,*,#5905,.F.);
#8054=ORIENTED_EDGE('',*,*,#5906,.T.);
#8055=ORIENTED_EDGE('',*,*,#5903,.T.);
#8056=ORIENTED_EDGE('',*,*,#5906,.F.);
#8057=ORIENTED_EDGE('',*,*,#5905,.T.);
#8058=ORIENTED_EDGE('',*,*,#5907,.F.);
#8059=ORIENTED_EDGE('',*,*,#5908,.F.);
#8060=ORIENTED_EDGE('',*,*,#5909,.T.);
#8061=ORIENTED_EDGE('',*,*,#5907,.T.);
#8062=ORIENTED_EDGE('',*,*,#5909,.F.);
#8063=ORIENTED_EDGE('',*,*,#5899,.T.);
#8064=ORIENTED_EDGE('',*,*,#5910,.T.);
#8065=ORIENTED_EDGE('',*,*,#5908,.T.);
#8066=ORIENTED_EDGE('',*,*,#5910,.F.);
#8067=CYLINDRICAL_SURFACE('',#9457,0.165);
#8068=CYLINDRICAL_SURFACE('',#9460,0.165);
#8069=CYLINDRICAL_SURFACE('',#9463,0.165);
#8070=CYLINDRICAL_SURFACE('',#9466,0.165);
#8071=CYLINDRICAL_SURFACE('',#9469,0.164999999999999);
#8072=CYLINDRICAL_SURFACE('',#9472,0.164999999999999);
#8073=CYLINDRICAL_SURFACE('',#9475,0.165);
#8074=CYLINDRICAL_SURFACE('',#9478,0.165);
#8075=CYLINDRICAL_SURFACE('',#9481,0.21);
#8076=CYLINDRICAL_SURFACE('',#9484,0.21);
#8077=CYLINDRICAL_SURFACE('',#9487,0.21);
#8078=CYLINDRICAL_SURFACE('',#9490,0.21);
#8079=CYLINDRICAL_SURFACE('',#9514,0.25);
#8080=CYLINDRICAL_SURFACE('',#9515,0.165);
#8081=CYLINDRICAL_SURFACE('',#9519,0.165);
#8082=CYLINDRICAL_SURFACE('',#9523,0.165);
#8083=CYLINDRICAL_SURFACE('',#9527,0.165);
#8084=CYLINDRICAL_SURFACE('',#9534,0.525);
#8085=CYLINDRICAL_SURFACE('',#9536,0.525);
#8086=CYLINDRICAL_SURFACE('',#9541,0.525);
#8087=CYLINDRICAL_SURFACE('',#9546,0.525);
#8088=CYLINDRICAL_SURFACE('',#9551,2.2);
#8089=CYLINDRICAL_SURFACE('',#9564,0.275);
#8090=CYLINDRICAL_SURFACE('',#9566,0.275);
#8091=CYLINDRICAL_SURFACE('',#9568,0.275);
#8092=CYLINDRICAL_SURFACE('',#9570,0.275);
#8093=CYLINDRICAL_SURFACE('',#9572,1.5);
#8094=CYLINDRICAL_SURFACE('',#9577,3.);
#8095=CYLINDRICAL_SURFACE('',#9579,1.02);
#8096=CYLINDRICAL_SURFACE('',#9584,0.375);
#8097=CYLINDRICAL_SURFACE('',#9589,0.375);
#8098=CYLINDRICAL_SURFACE('',#9594,0.375);
#8099=CYLINDRICAL_SURFACE('',#9599,0.375);
#8100=CYLINDRICAL_SURFACE('',#9604,0.225);
#8101=CYLINDRICAL_SURFACE('',#9606,0.225);
#8102=CYLINDRICAL_SURFACE('',#9608,0.225);
#8103=CYLINDRICAL_SURFACE('',#9610,0.225);
#8104=CYLINDRICAL_SURFACE('',#9612,1.49);
#8105=CYLINDRICAL_SURFACE('',#9617,0.71);
#8106=CYLINDRICAL_SURFACE('',#9619,2.2);
#8107=CYLINDRICAL_SURFACE('',#9625,0.4);
#8108=CYLINDRICAL_SURFACE('',#9628,0.4);
#8109=CYLINDRICAL_SURFACE('',#9633,0.165);
#8110=CYLINDRICAL_SURFACE('',#9637,0.4);
#8111=CYLINDRICAL_SURFACE('',#9642,0.4);
#8112=CYLINDRICAL_SURFACE('',#9648,0.225);
#8113=CYLINDRICAL_SURFACE('',#9650,0.225);
#8114=CYLINDRICAL_SURFACE('',#9652,0.6);
#8115=CYLINDRICAL_SURFACE('',#9661,0.4);
#8116=CYLINDRICAL_SURFACE('',#9664,0.4);
#8117=CYLINDRICAL_SURFACE('',#9669,0.164999999999999);
#8118=CYLINDRICAL_SURFACE('',#9673,0.4);
#8119=CYLINDRICAL_SURFACE('',#9678,0.4);
#8120=CYLINDRICAL_SURFACE('',#9684,0.225);
#8121=CYLINDRICAL_SURFACE('',#9686,0.225);
#8122=CYLINDRICAL_SURFACE('',#9688,0.6);
#8123=CYLINDRICAL_SURFACE('',#9697,0.4);
#8124=CYLINDRICAL_SURFACE('',#9702,0.165);
#8125=CYLINDRICAL_SURFACE('',#9707,0.4);
#8126=CYLINDRICAL_SURFACE('',#9712,0.4);
#8127=CYLINDRICAL_SURFACE('',#9718,0.225);
#8128=CYLINDRICAL_SURFACE('',#9720,0.225);
#8129=CYLINDRICAL_SURFACE('',#9722,0.6);
#8130=CYLINDRICAL_SURFACE('',#9731,0.4);
#8131=CYLINDRICAL_SURFACE('',#9736,0.165);
#8132=CYLINDRICAL_SURFACE('',#9741,0.4);
#8133=CYLINDRICAL_SURFACE('',#9746,0.4);
#8134=CYLINDRICAL_SURFACE('',#9752,0.225);
#8135=CYLINDRICAL_SURFACE('',#9754,0.225);
#8136=CYLINDRICAL_SURFACE('',#9756,0.6);
#8137=CYLINDRICAL_SURFACE('',#9779,0.425);
#8138=CYLINDRICAL_SURFACE('',#9787,0.24505);
#8139=CYLINDRICAL_SURFACE('',#9796,0.976185);
#8140=CYLINDRICAL_SURFACE('',#9798,0.5);
#8141=CYLINDRICAL_SURFACE('',#9804,0.976185);
#8142=CYLINDRICAL_SURFACE('',#9816,1.023815);
#8143=CYLINDRICAL_SURFACE('',#9823,1.5);
#8144=CYLINDRICAL_SURFACE('',#9828,1.023815);
#8145=CYLINDRICAL_SURFACE('',#9850,1.019052);
#8146=CYLINDRICAL_SURFACE('',#9890,0.980948);
#8147=CYLINDRICAL_SURFACE('',#9904,1.013815);
#8148=CYLINDRICAL_SURFACE('',#9908,0.991185);
#8149=CYLINDRICAL_SURFACE('',#9912,1.013815);
#8150=CYLINDRICAL_SURFACE('',#9916,0.991185);
#8151=CYLINDRICAL_SURFACE('',#9928,0.6);
#8152=CYLINDRICAL_SURFACE('',#9942,0.1954);
#8153=CYLINDRICAL_SURFACE('',#9949,0.25);
#8154=CYLINDRICAL_SURFACE('',#9952,0.25);
#8155=CYLINDRICAL_SURFACE('',#9955,0.225);
#8156=CYLINDRICAL_SURFACE('',#9958,0.8);
#8157=CYLINDRICAL_SURFACE('',#9969,1.);
#8158=CYLINDRICAL_SURFACE('',#9971,1.);
#8159=CYLINDRICAL_SURFACE('',#9973,0.8);
#8160=CYLINDRICAL_SURFACE('',#9981,0.8);
#8161=CYLINDRICAL_SURFACE('',#9984,1.);
#8162=CYLINDRICAL_SURFACE('',#9988,0.7);
#8163=CYLINDRICAL_SURFACE('',#9989,0.5);
#8164=CYLINDRICAL_SURFACE('',#9993,0.165);
#8165=CYLINDRICAL_SURFACE('',#9997,0.6);
#8166=CYLINDRICAL_SURFACE('',#10003,0.505);
#8167=CYLINDRICAL_SURFACE('',#10006,0.7);
#8168=CYLINDRICAL_SURFACE('',#10014,0.165);
#8169=CYLINDRICAL_SURFACE('',#10017,0.505);
#8170=CYLINDRICAL_SURFACE('',#10020,0.9);
#8171=CYLINDRICAL_SURFACE('',#10026,0.165);
#8172=CYLINDRICAL_SURFACE('',#10036,0.7);
#8173=CYLINDRICAL_SURFACE('',#10037,0.3);
#8174=CYLINDRICAL_SURFACE('',#10039,0.3);
#8175=CYLINDRICAL_SURFACE('',#10044,0.305);
#8176=CYLINDRICAL_SURFACE('',#10047,0.5);
#8177=CYLINDRICAL_SURFACE('',#10053,0.305);
#8178=CYLINDRICAL_SURFACE('',#10056,0.5);
#8179=CYLINDRICAL_SURFACE('',#10062,0.225);
#8180=CYLINDRICAL_SURFACE('',#10065,0.5);
#8181=CYLINDRICAL_SURFACE('',#10071,0.165);
#8182=CYLINDRICAL_SURFACE('',#10081,0.7);
#8183=CYLINDRICAL_SURFACE('',#10082,0.3);
#8184=CYLINDRICAL_SURFACE('',#10084,0.3);
#8185=CYLINDRICAL_SURFACE('',#10089,0.305);
#8186=CYLINDRICAL_SURFACE('',#10092,0.5);
#8187=CYLINDRICAL_SURFACE('',#10098,0.305);
#8188=CYLINDRICAL_SURFACE('',#10101,0.5);
#8189=CYLINDRICAL_SURFACE('',#10107,0.225);
#8190=CYLINDRICAL_SURFACE('',#10110,0.5);
#8191=CYLINDRICAL_SURFACE('',#10120,0.35);
#8192=CYLINDRICAL_SURFACE('',#10128,0.1954);
#8193=CYLINDRICAL_SURFACE('',#10155,0.1954);
#8194=CYLINDRICAL_SURFACE('',#10158,0.5);
#8195=CYLINDRICAL_SURFACE('',#10161,0.5);
#8196=CYLINDRICAL_SURFACE('',#10164,0.800000000000001);
#8197=CYLINDRICAL_SURFACE('',#10171,0.8);
#8198=CYLINDRICAL_SURFACE('',#10175,0.305);
#8199=CYLINDRICAL_SURFACE('',#10178,0.5);
#8200=CYLINDRICAL_SURFACE('',#10184,0.305);
#8201=CYLINDRICAL_SURFACE('',#10187,0.5);
#8202=CYLINDRICAL_SURFACE('',#10197,0.5);
#8203=CYLINDRICAL_SURFACE('',#10200,0.5);
#8204=CYLINDRICAL_SURFACE('',#10203,0.8);
#8205=CYLINDRICAL_SURFACE('',#10210,0.8);
#8206=CYLINDRICAL_SURFACE('',#10214,0.305);
#8207=CYLINDRICAL_SURFACE('',#10217,0.5);
#8208=CYLINDRICAL_SURFACE('',#10223,0.305);
#8209=CYLINDRICAL_SURFACE('',#10226,0.5);
#8210=CYLINDRICAL_SURFACE('',#10236,0.25);
#8211=CYLINDRICAL_SURFACE('',#10240,0.165);
#8212=CYLINDRICAL_SURFACE('',#10243,0.165);
#8213=CYLINDRICAL_SURFACE('',#10246,0.165);
#8214=CYLINDRICAL_SURFACE('',#10249,0.165);
#8215=CYLINDRICAL_SURFACE('',#10252,1.05);
#8216=CYLINDRICAL_SURFACE('',#10262,0.225);
#8217=CYLINDRICAL_SURFACE('',#10265,0.225);
#8218=CYLINDRICAL_SURFACE('',#10268,0.225);
#8219=CYLINDRICAL_SURFACE('',#10271,0.225);
#8220=CYLINDRICAL_SURFACE('',#10274,0.7);
#8221=CYLINDRICAL_SURFACE('',#10284,0.225);
#8222=CYLINDRICAL_SURFACE('',#10287,0.225);
#8223=CYLINDRICAL_SURFACE('',#10290,0.225);
#8224=CYLINDRICAL_SURFACE('',#10293,0.225);
#8225=CYLINDRICAL_SURFACE('',#10296,0.7);
#8226=CYLINDRICAL_SURFACE('',#10306,0.164999999999999);
#8227=CYLINDRICAL_SURFACE('',#10316,0.699999999999999);
#8228=CYLINDRICAL_SURFACE('',#10317,0.300000000000001);
#8229=CYLINDRICAL_SURFACE('',#10319,0.300000000000001);
#8230=CYLINDRICAL_SURFACE('',#10324,0.305);
#8231=CYLINDRICAL_SURFACE('',#10327,0.5);
#8232=CYLINDRICAL_SURFACE('',#10333,0.305);
#8233=CYLINDRICAL_SURFACE('',#10336,0.5);
#8234=CYLINDRICAL_SURFACE('',#10342,0.225);
#8235=CYLINDRICAL_SURFACE('',#10345,0.5);
#8236=CYLINDRICAL_SURFACE('',#10352,0.25);
#8237=CYLINDRICAL_SURFACE('',#10356,0.165);
#8238=CYLINDRICAL_SURFACE('',#10359,0.165);
#8239=CYLINDRICAL_SURFACE('',#10362,0.165);
#8240=CYLINDRICAL_SURFACE('',#10365,0.165);
#8241=CYLINDRICAL_SURFACE('',#10368,1.05);
#8242=CYLINDRICAL_SURFACE('',#10378,0.225);
#8243=CYLINDRICAL_SURFACE('',#10381,0.225);
#8244=CYLINDRICAL_SURFACE('',#10384,0.225);
#8245=CYLINDRICAL_SURFACE('',#10387,0.225);
#8246=CYLINDRICAL_SURFACE('',#10390,0.7);
#8247=CYLINDRICAL_SURFACE('',#10400,0.225);
#8248=CYLINDRICAL_SURFACE('',#10403,0.225);
#8249=CYLINDRICAL_SURFACE('',#10406,0.225);
#8250=CYLINDRICAL_SURFACE('',#10409,0.225);
#8251=CYLINDRICAL_SURFACE('',#10412,0.7);
#8252=CYLINDRICAL_SURFACE('',#10422,0.165);
#8253=CYLINDRICAL_SURFACE('',#10432,0.7);
#8254=CYLINDRICAL_SURFACE('',#10433,0.3);
#8255=CYLINDRICAL_SURFACE('',#10435,0.3);
#8256=CYLINDRICAL_SURFACE('',#10440,0.305);
#8257=CYLINDRICAL_SURFACE('',#10443,0.5);
#8258=CYLINDRICAL_SURFACE('',#10449,0.305);
#8259=CYLINDRICAL_SURFACE('',#10452,0.5);
#8260=CYLINDRICAL_SURFACE('',#10458,0.225);
#8261=CYLINDRICAL_SURFACE('',#10461,0.5);
#8262=CYLINDRICAL_SURFACE('',#10478,1.05);
#8263=CYLINDRICAL_SURFACE('',#10482,1.);
#8264=CYLINDRICAL_SURFACE('',#10486,1.05);
#8265=CYLINDRICAL_SURFACE('',#10490,1.);
#8266=CYLINDRICAL_SURFACE('',#10494,1.05);
#8267=CYLINDRICAL_SURFACE('',#10498,0.9);
#8268=CYLINDRICAL_SURFACE('',#10511,0.895);
#8269=CYLINDRICAL_SURFACE('',#10515,0.605);
#8270=CYLINDRICAL_SURFACE('',#10533,0.35);
#8271=CYLINDRICAL_SURFACE('',#10541,0.1954);
#8272=ADVANCED_FACE('',(#1247),#8067,.F.);
#8273=ADVANCED_FACE('',(#1248),#8068,.F.);
#8274=ADVANCED_FACE('',(#1249),#8069,.F.);
#8275=ADVANCED_FACE('',(#1250),#8070,.F.);
#8276=ADVANCED_FACE('',(#1251),#8071,.F.);
#8277=ADVANCED_FACE('',(#1252),#8072,.F.);
#8278=ADVANCED_FACE('',(#1253),#8073,.F.);
#8279=ADVANCED_FACE('',(#1254),#8074,.F.);
#8280=ADVANCED_FACE('',(#1255),#8075,.F.);
#8281=ADVANCED_FACE('',(#1256),#8076,.F.);
#8282=ADVANCED_FACE('',(#1257),#8077,.F.);
#8283=ADVANCED_FACE('',(#1258),#8078,.F.);
#8284=ADVANCED_FACE('',(#1259),#966,.T.);
#8285=ADVANCED_FACE('',(#1260),#967,.T.);
#8286=ADVANCED_FACE('',(#1261),#968,.T.);
#8287=ADVANCED_FACE('',(#1262),#969,.T.);
#8288=ADVANCED_FACE('',(#1263,#725,#726,#727,#728,#729,#730,#731,#732,#733,
#734,#735,#736),#970,.T.);
#8289=ADVANCED_FACE('',(#1264,#737,#738,#739,#740,#741,#742,#743,#744,#745,
#746,#747,#748),#971,.F.);
#8290=ADVANCED_FACE('',(#1265),#972,.T.);
#8291=ADVANCED_FACE('',(#1266),#973,.T.);
#8292=ADVANCED_FACE('',(#1267),#974,.T.);
#8293=ADVANCED_FACE('',(#1268),#975,.T.);
#8294=ADVANCED_FACE('',(#1269),#976,.T.);
#8295=ADVANCED_FACE('',(#1270),#977,.F.);
#8296=ADVANCED_FACE('',(#1271),#978,.T.);
#8297=ADVANCED_FACE('',(#1272),#979,.T.);
#8298=ADVANCED_FACE('',(#1273),#980,.T.);
#8299=ADVANCED_FACE('',(#1274),#981,.T.);
#8300=ADVANCED_FACE('',(#1275),#982,.T.);
#8301=ADVANCED_FACE('',(#1276),#983,.F.);
#8302=ADVANCED_FACE('',(#1277),#8079,.F.);
#8303=ADVANCED_FACE('',(#1278),#8080,.F.);
#8304=ADVANCED_FACE('',(#1279),#984,.T.);
#8305=ADVANCED_FACE('',(#1280),#8081,.F.);
#8306=ADVANCED_FACE('',(#1281),#985,.T.);
#8307=ADVANCED_FACE('',(#1282),#8082,.F.);
#8308=ADVANCED_FACE('',(#1283),#986,.T.);
#8309=ADVANCED_FACE('',(#1284),#8083,.F.);
#8310=ADVANCED_FACE('',(#1285),#987,.T.);
#8311=ADVANCED_FACE('',(#1286),#988,.F.);
#8312=ADVANCED_FACE('',(#1287),#8084,.F.);
#8313=ADVANCED_FACE('',(#1288),#8085,.F.);
#8314=ADVANCED_FACE('',(#1289),#989,.F.);
#8315=ADVANCED_FACE('',(#1290),#8086,.F.);
#8316=ADVANCED_FACE('',(#1291),#990,.F.);
#8317=ADVANCED_FACE('',(#1292),#8087,.F.);
#8318=ADVANCED_FACE('',(#1293),#991,.F.);
#8319=ADVANCED_FACE('',(#1294),#8088,.T.);
#8320=ADVANCED_FACE('',(#1295,#749,#750,#751,#752,#753),#992,.T.);
#8321=ADVANCED_FACE('',(#1296),#8089,.F.);
#8322=ADVANCED_FACE('',(#1297),#8090,.F.);
#8323=ADVANCED_FACE('',(#1298),#8091,.F.);
#8324=ADVANCED_FACE('',(#1299),#8092,.F.);
#8325=ADVANCED_FACE('',(#1300),#8093,.F.);
#8326=ADVANCED_FACE('',(#1301,#754),#993,.T.);
#8327=ADVANCED_FACE('',(#1302,#755),#8094,.T.);
#8328=ADVANCED_FACE('',(#1303,#756),#8095,.F.);
#8329=ADVANCED_FACE('',(#1304,#757,#758,#759,#760,#761),#994,.T.);
#8330=ADVANCED_FACE('',(#1305,#762,#763,#764,#765,#766),#995,.F.);
#8331=ADVANCED_FACE('',(#1306),#8096,.F.);
#8332=ADVANCED_FACE('',(#1307,#767),#996,.T.);
#8333=ADVANCED_FACE('',(#1308),#8097,.F.);
#8334=ADVANCED_FACE('',(#1309,#768),#997,.T.);
#8335=ADVANCED_FACE('',(#1310),#8098,.F.);
#8336=ADVANCED_FACE('',(#1311,#769),#998,.T.);
#8337=ADVANCED_FACE('',(#1312),#8099,.F.);
#8338=ADVANCED_FACE('',(#1313,#770),#999,.T.);
#8339=ADVANCED_FACE('',(#1314),#8100,.F.);
#8340=ADVANCED_FACE('',(#1315),#8101,.F.);
#8341=ADVANCED_FACE('',(#1316),#8102,.F.);
#8342=ADVANCED_FACE('',(#1317),#8103,.F.);
#8343=ADVANCED_FACE('',(#1318),#8104,.T.);
#8344=ADVANCED_FACE('',(#1319,#771),#1000,.F.);
#8345=ADVANCED_FACE('',(#1320),#8105,.F.);
#8346=ADVANCED_FACE('',(#1321),#8106,.T.);
#8347=ADVANCED_FACE('',(#1322,#772,#773,#774,#775,#776),#1001,.T.);
#8348=ADVANCED_FACE('',(#1323,#777,#778,#779,#780,#781),#1002,.F.);
#8349=ADVANCED_FACE('',(#1324),#8107,.F.);
#8350=ADVANCED_FACE('',(#1325),#8108,.F.);
#8351=ADVANCED_FACE('',(#1326),#1003,.T.);
#8352=ADVANCED_FACE('',(#1327),#8109,.F.);
#8353=ADVANCED_FACE('',(#1328),#1004,.T.);
#8354=ADVANCED_FACE('',(#1329),#8110,.F.);
#8355=ADVANCED_FACE('',(#1330,#782),#1005,.T.);
#8356=ADVANCED_FACE('',(#1331),#8111,.F.);
#8357=ADVANCED_FACE('',(#1332,#783),#1006,.T.);
#8358=ADVANCED_FACE('',(#1333,#784),#1007,.T.);
#8359=ADVANCED_FACE('',(#1334),#8112,.F.);
#8360=ADVANCED_FACE('',(#1335),#8113,.F.);
#8361=ADVANCED_FACE('',(#1336),#8114,.F.);
#8362=ADVANCED_FACE('',(#1337),#1008,.T.);
#8363=ADVANCED_FACE('',(#1338,#785),#1009,.T.);
#8364=ADVANCED_FACE('',(#1339),#1010,.T.);
#8365=ADVANCED_FACE('',(#1340,#786),#1011,.T.);
#8366=ADVANCED_FACE('',(#1341,#787,#788),#1012,.F.);
#8367=ADVANCED_FACE('',(#1342),#8115,.F.);
#8368=ADVANCED_FACE('',(#1343),#8116,.F.);
#8369=ADVANCED_FACE('',(#1344),#1013,.T.);
#8370=ADVANCED_FACE('',(#1345),#8117,.F.);
#8371=ADVANCED_FACE('',(#1346),#1014,.T.);
#8372=ADVANCED_FACE('',(#1347),#8118,.F.);
#8373=ADVANCED_FACE('',(#1348,#789),#1015,.T.);
#8374=ADVANCED_FACE('',(#1349),#8119,.F.);
#8375=ADVANCED_FACE('',(#1350,#790),#1016,.T.);
#8376=ADVANCED_FACE('',(#1351,#791),#1017,.T.);
#8377=ADVANCED_FACE('',(#1352),#8120,.F.);
#8378=ADVANCED_FACE('',(#1353),#8121,.F.);
#8379=ADVANCED_FACE('',(#1354),#8122,.F.);
#8380=ADVANCED_FACE('',(#1355),#1018,.T.);
#8381=ADVANCED_FACE('',(#1356,#792),#1019,.T.);
#8382=ADVANCED_FACE('',(#1357),#1020,.T.);
#8383=ADVANCED_FACE('',(#1358,#793),#1021,.T.);
#8384=ADVANCED_FACE('',(#1359,#794,#795),#1022,.F.);
#8385=ADVANCED_FACE('',(#1360),#8123,.F.);
#8386=ADVANCED_FACE('',(#1361),#1023,.T.);
#8387=ADVANCED_FACE('',(#1362),#8124,.F.);
#8388=ADVANCED_FACE('',(#1363),#1024,.T.);
#8389=ADVANCED_FACE('',(#1364),#8125,.F.);
#8390=ADVANCED_FACE('',(#1365,#796),#1025,.T.);
#8391=ADVANCED_FACE('',(#1366),#8126,.F.);
#8392=ADVANCED_FACE('',(#1367,#797),#1026,.T.);
#8393=ADVANCED_FACE('',(#1368,#798),#1027,.T.);
#8394=ADVANCED_FACE('',(#1369),#8127,.F.);
#8395=ADVANCED_FACE('',(#1370),#8128,.F.);
#8396=ADVANCED_FACE('',(#1371,#799),#8129,.F.);
#8397=ADVANCED_FACE('',(#1372,#800),#1028,.T.);
#8398=ADVANCED_FACE('',(#1373),#1029,.T.);
#8399=ADVANCED_FACE('',(#1374,#801),#1030,.T.);
#8400=ADVANCED_FACE('',(#1375),#1031,.T.);
#8401=ADVANCED_FACE('',(#1376,#802,#803),#1032,.F.);
#8402=ADVANCED_FACE('',(#1377),#8130,.F.);
#8403=ADVANCED_FACE('',(#1378),#1033,.T.);
#8404=ADVANCED_FACE('',(#1379),#8131,.F.);
#8405=ADVANCED_FACE('',(#1380),#1034,.T.);
#8406=ADVANCED_FACE('',(#1381),#8132,.F.);
#8407=ADVANCED_FACE('',(#1382,#804),#1035,.T.);
#8408=ADVANCED_FACE('',(#1383),#8133,.F.);
#8409=ADVANCED_FACE('',(#1384,#805),#1036,.T.);
#8410=ADVANCED_FACE('',(#1385,#806),#1037,.T.);
#8411=ADVANCED_FACE('',(#1386),#8134,.F.);
#8412=ADVANCED_FACE('',(#1387),#8135,.F.);
#8413=ADVANCED_FACE('',(#1388,#807),#8136,.F.);
#8414=ADVANCED_FACE('',(#1389,#808),#1038,.T.);
#8415=ADVANCED_FACE('',(#1390),#1039,.T.);
#8416=ADVANCED_FACE('',(#1391,#809),#1040,.T.);
#8417=ADVANCED_FACE('',(#1392),#1041,.T.);
#8418=ADVANCED_FACE('',(#1393,#810,#811),#1042,.F.);
#8419=ADVANCED_FACE('',(#1394),#1043,.F.);
#8420=ADVANCED_FACE('',(#1395),#1044,.F.);
#8421=ADVANCED_FACE('',(#1396),#1045,.F.);
#8422=ADVANCED_FACE('',(#1397),#1046,.F.);
#8423=ADVANCED_FACE('',(#1398),#1047,.F.);
#8424=ADVANCED_FACE('',(#1399),#1048,.F.);
#8425=ADVANCED_FACE('',(#1400),#1049,.F.);
#8426=ADVANCED_FACE('',(#1401),#1050,.F.);
#8427=ADVANCED_FACE('',(#1402),#1051,.F.);
#8428=ADVANCED_FACE('',(#1403),#1052,.T.);
#8429=ADVANCED_FACE('',(#1404),#433,.T.);
#8430=ADVANCED_FACE('',(#1405),#8137,.T.);
#8431=ADVANCED_FACE('',(#1406),#434,.T.);
#8432=ADVANCED_FACE('',(#1407,#812),#1053,.T.);
#8433=ADVANCED_FACE('',(#1408),#435,.T.);
#8434=ADVANCED_FACE('',(#1409),#8138,.T.);
#8435=ADVANCED_FACE('',(#1410),#431,.F.);
#8436=ADVANCED_FACE('',(#1411),#8139,.T.);
#8437=ADVANCED_FACE('',(#1412),#8140,.F.);
#8438=ADVANCED_FACE('',(#1413),#436,.F.);
#8439=ADVANCED_FACE('',(#1414,#813),#1054,.T.);
#8440=ADVANCED_FACE('',(#1415),#8141,.T.);
#8441=ADVANCED_FACE('',(#1416,#814),#1055,.T.);
#8442=ADVANCED_FACE('',(#1417),#437,.F.);
#8443=ADVANCED_FACE('',(#1418),#432,.F.);
#8444=ADVANCED_FACE('',(#1419),#8142,.F.);
#8445=ADVANCED_FACE('',(#1420,#815),#1056,.T.);
#8446=ADVANCED_FACE('',(#1421),#438,.T.);
#8447=ADVANCED_FACE('',(#1422),#8143,.T.);
#8448=ADVANCED_FACE('',(#1423),#439,.T.);
#8449=ADVANCED_FACE('',(#1424,#816),#1057,.T.);
#8450=ADVANCED_FACE('',(#1425),#8144,.F.);
#8451=ADVANCED_FACE('',(#1426),#415,.T.);
#8452=ADVANCED_FACE('',(#1427),#416,.T.);
#8453=ADVANCED_FACE('',(#1428),#417,.T.);
#8454=ADVANCED_FACE('',(#1429),#418,.T.);
#8455=ADVANCED_FACE('',(#1430),#419,.T.);
#8456=ADVANCED_FACE('',(#1431),#420,.T.);
#8457=ADVANCED_FACE('',(#1432),#421,.T.);
#8458=ADVANCED_FACE('',(#1433),#422,.T.);
#8459=ADVANCED_FACE('',(#1434),#423,.F.);
#8460=ADVANCED_FACE('',(#1435),#8145,.T.);
#8461=ADVANCED_FACE('',(#1436),#1058,.T.);
#8462=ADVANCED_FACE('',(#1437),#424,.F.);
#8463=ADVANCED_FACE('',(#1438),#1059,.T.);
#8464=ADVANCED_FACE('',(#1439),#425,.F.);
#8465=ADVANCED_FACE('',(#1440),#1060,.T.);
#8466=ADVANCED_FACE('',(#1441),#426,.F.);
#8467=ADVANCED_FACE('',(#1442),#1061,.T.);
#8468=ADVANCED_FACE('',(#1443),#427,.F.);
#8469=ADVANCED_FACE('',(#1444),#1062,.T.);
#8470=ADVANCED_FACE('',(#1445),#428,.F.);
#8471=ADVANCED_FACE('',(#1446),#1063,.T.);
#8472=ADVANCED_FACE('',(#1447),#429,.F.);
#8473=ADVANCED_FACE('',(#1448),#8146,.F.);
#8474=ADVANCED_FACE('',(#1449),#1064,.T.);
#8475=ADVANCED_FACE('',(#1450),#430,.F.);
#8476=ADVANCED_FACE('',(#1451,#817),#1065,.T.);
#8477=ADVANCED_FACE('',(#1452),#1066,.T.);
#8478=ADVANCED_FACE('',(#1453,#818),#1067,.T.);
#8479=ADVANCED_FACE('',(#1454),#8147,.T.);
#8480=ADVANCED_FACE('',(#1455,#819),#1068,.T.);
#8481=ADVANCED_FACE('',(#1456),#8148,.F.);
#8482=ADVANCED_FACE('',(#1457,#820),#1069,.T.);
#8483=ADVANCED_FACE('',(#1458),#8149,.T.);
#8484=ADVANCED_FACE('',(#1459,#821),#1070,.T.);
#8485=ADVANCED_FACE('',(#1460),#8150,.F.);
#8486=ADVANCED_FACE('',(#1461),#1071,.T.);
#8487=ADVANCED_FACE('',(#1462),#440,.T.);
#8488=ADVANCED_FACE('',(#1463),#8151,.T.);
#8489=ADVANCED_FACE('',(#1464),#1072,.F.);
#8490=ADVANCED_FACE('',(#1465),#1073,.F.);
#8491=ADVANCED_FACE('',(#1466),#1074,.F.);
#8492=ADVANCED_FACE('',(#1467),#1075,.F.);
#8493=ADVANCED_FACE('',(#1468),#1076,.F.);
#8494=ADVANCED_FACE('',(#1469),#1077,.F.);
#8495=ADVANCED_FACE('',(#1470),#1078,.F.);
#8496=ADVANCED_FACE('',(#1471),#1079,.F.);
#8497=ADVANCED_FACE('',(#1472,#822),#1080,.T.);
#8498=ADVANCED_FACE('',(#1473),#441,.T.);
#8499=ADVANCED_FACE('',(#1474),#8152,.T.);
#8500=ADVANCED_FACE('',(#1475),#442,.T.);
#8501=ADVANCED_FACE('',(#1476),#1081,.T.);
#8502=ADVANCED_FACE('',(#1477),#8153,.F.);
#8503=ADVANCED_FACE('',(#1478),#8154,.F.);
#8504=ADVANCED_FACE('',(#1479),#8155,.F.);
#8505=ADVANCED_FACE('',(#1480),#8156,.T.);
#8506=ADVANCED_FACE('',(#1481),#1082,.T.);
#8507=ADVANCED_FACE('',(#1482,#823,#824,#825),#1083,.T.);
#8508=ADVANCED_FACE('',(#1483),#1084,.T.);
#8509=ADVANCED_FACE('',(#1484),#8157,.T.);
#8510=ADVANCED_FACE('',(#1485),#8158,.T.);
#8511=ADVANCED_FACE('',(#1486),#8159,.T.);
#8512=ADVANCED_FACE('',(#1487),#1085,.T.);
#8513=ADVANCED_FACE('',(#1488,#826,#827,#828,#829),#1086,.F.);
#8514=ADVANCED_FACE('',(#1489),#1087,.T.);
#8515=ADVANCED_FACE('',(#1490),#8160,.T.);
#8516=ADVANCED_FACE('',(#1491),#1088,.T.);
#8517=ADVANCED_FACE('',(#1492),#1089,.T.);
#8518=ADVANCED_FACE('',(#1493),#8161,.T.);
#8519=ADVANCED_FACE('',(#1494,#830),#1090,.F.);
#8520=ADVANCED_FACE('',(#1495),#8162,.T.);
#8521=ADVANCED_FACE('',(#1496),#8163,.T.);
#8522=ADVANCED_FACE('',(#1497),#1091,.F.);
#8523=ADVANCED_FACE('',(#1498),#8164,.F.);
#8524=ADVANCED_FACE('',(#1499),#1092,.F.);
#8525=ADVANCED_FACE('',(#1500),#8165,.T.);
#8526=ADVANCED_FACE('',(#1501),#1093,.T.);
#8527=ADVANCED_FACE('',(#1502,#831),#1094,.F.);
#8528=ADVANCED_FACE('',(#1503),#8166,.F.);
#8529=ADVANCED_FACE('',(#1504),#8167,.T.);
#8530=ADVANCED_FACE('',(#1505,#832),#1095,.T.);
#8531=ADVANCED_FACE('',(#1506,#833),#1096,.F.);
#8532=ADVANCED_FACE('',(#1507),#1097,.T.);
#8533=ADVANCED_FACE('',(#1508),#8168,.F.);
#8534=ADVANCED_FACE('',(#1509),#1098,.T.);
#8535=ADVANCED_FACE('',(#1510,#834),#8169,.F.);
#8536=ADVANCED_FACE('',(#1511,#835),#8170,.T.);
#8537=ADVANCED_FACE('',(#1512,#836),#1099,.T.);
#8538=ADVANCED_FACE('',(#1513,#837),#1100,.F.);
#8539=ADVANCED_FACE('',(#1514),#8171,.F.);
#8540=ADVANCED_FACE('',(#1515),#1101,.T.);
#8541=ADVANCED_FACE('',(#1516,#838),#1102,.T.);
#8542=ADVANCED_FACE('',(#1517,#839),#1103,.F.);
#8543=ADVANCED_FACE('',(#1518),#8172,.T.);
#8544=ADVANCED_FACE('',(#1519),#8173,.T.);
#8545=ADVANCED_FACE('',(#1520),#8174,.T.);
#8546=ADVANCED_FACE('',(#1521,#840),#1104,.T.);
#8547=ADVANCED_FACE('',(#1522),#1105,.F.);
#8548=ADVANCED_FACE('',(#1523),#8175,.F.);
#8549=ADVANCED_FACE('',(#1524),#8176,.T.);
#8550=ADVANCED_FACE('',(#1525,#841),#1106,.T.);
#8551=ADVANCED_FACE('',(#1526,#842),#1107,.F.);
#8552=ADVANCED_FACE('',(#1527),#8177,.F.);
#8553=ADVANCED_FACE('',(#1528),#8178,.T.);
#8554=ADVANCED_FACE('',(#1529,#843),#1108,.T.);
#8555=ADVANCED_FACE('',(#1530,#844),#1109,.F.);
#8556=ADVANCED_FACE('',(#1531),#8179,.F.);
#8557=ADVANCED_FACE('',(#1532),#8180,.T.);
#8558=ADVANCED_FACE('',(#1533,#845),#1110,.T.);
#8559=ADVANCED_FACE('',(#1534,#846),#1111,.F.);
#8560=ADVANCED_FACE('',(#1535),#8181,.F.);
#8561=ADVANCED_FACE('',(#1536),#1112,.T.);
#8562=ADVANCED_FACE('',(#1537,#847),#1113,.T.);
#8563=ADVANCED_FACE('',(#1538,#848),#1114,.F.);
#8564=ADVANCED_FACE('',(#1539),#8182,.T.);
#8565=ADVANCED_FACE('',(#1540),#8183,.T.);
#8566=ADVANCED_FACE('',(#1541),#8184,.T.);
#8567=ADVANCED_FACE('',(#1542,#849),#1115,.T.);
#8568=ADVANCED_FACE('',(#1543),#1116,.F.);
#8569=ADVANCED_FACE('',(#1544),#8185,.F.);
#8570=ADVANCED_FACE('',(#1545),#8186,.T.);
#8571=ADVANCED_FACE('',(#1546,#850),#1117,.T.);
#8572=ADVANCED_FACE('',(#1547,#851),#1118,.F.);
#8573=ADVANCED_FACE('',(#1548),#8187,.F.);
#8574=ADVANCED_FACE('',(#1549),#8188,.T.);
#8575=ADVANCED_FACE('',(#1550,#852),#1119,.T.);
#8576=ADVANCED_FACE('',(#1551,#853),#1120,.F.);
#8577=ADVANCED_FACE('',(#1552),#8189,.F.);
#8578=ADVANCED_FACE('',(#1553),#8190,.T.);
#8579=ADVANCED_FACE('',(#1554,#854),#1121,.T.);
#8580=ADVANCED_FACE('',(#1555,#855),#1122,.F.);
#8581=ADVANCED_FACE('',(#1556),#1123,.T.);
#8582=ADVANCED_FACE('',(#1557),#443,.T.);
#8583=ADVANCED_FACE('',(#1558),#8191,.T.);
#8584=ADVANCED_FACE('',(#1559),#444,.T.);
#8585=ADVANCED_FACE('',(#1560,#856),#1124,.T.);
#8586=ADVANCED_FACE('',(#1561),#445,.T.);
#8587=ADVANCED_FACE('',(#1562),#8192,.T.);
#8588=ADVANCED_FACE('',(#1563),#446,.T.);
#8589=ADVANCED_FACE('',(#1564),#1125,.T.);
#8590=ADVANCED_FACE('',(#1565),#1126,.F.);
#8591=ADVANCED_FACE('',(#1566),#1127,.F.);
#8592=ADVANCED_FACE('',(#1567),#1128,.F.);
#8593=ADVANCED_FACE('',(#1568),#1129,.F.);
#8594=ADVANCED_FACE('',(#1569),#1130,.F.);
#8595=ADVANCED_FACE('',(#1570),#1131,.F.);
#8596=ADVANCED_FACE('',(#1571),#1132,.F.);
#8597=ADVANCED_FACE('',(#1572),#1133,.F.);
#8598=ADVANCED_FACE('',(#1573),#1134,.F.);
#8599=ADVANCED_FACE('',(#1574),#1135,.F.);
#8600=ADVANCED_FACE('',(#1575),#1136,.F.);
#8601=ADVANCED_FACE('',(#1576),#1137,.F.);
#8602=ADVANCED_FACE('',(#1577),#1138,.F.);
#8603=ADVANCED_FACE('',(#1578),#1139,.F.);
#8604=ADVANCED_FACE('',(#1579),#1140,.F.);
#8605=ADVANCED_FACE('',(#1580),#1141,.F.);
#8606=ADVANCED_FACE('',(#1581,#857),#1142,.T.);
#8607=ADVANCED_FACE('',(#1582),#447,.T.);
#8608=ADVANCED_FACE('',(#1583),#8193,.T.);
#8609=ADVANCED_FACE('',(#1584),#8194,.F.);
#8610=ADVANCED_FACE('',(#1585),#8195,.F.);
#8611=ADVANCED_FACE('',(#1586),#8196,.T.);
#8612=ADVANCED_FACE('',(#1587),#1143,.T.);
#8613=ADVANCED_FACE('',(#1588,#858,#859),#1144,.F.);
#8614=ADVANCED_FACE('',(#1589),#1145,.T.);
#8615=ADVANCED_FACE('',(#1590),#8197,.T.);
#8616=ADVANCED_FACE('',(#1591,#860,#861),#1146,.T.);
#8617=ADVANCED_FACE('',(#1592),#8198,.F.);
#8618=ADVANCED_FACE('',(#1593),#8199,.T.);
#8619=ADVANCED_FACE('',(#1594,#862),#1147,.T.);
#8620=ADVANCED_FACE('',(#1595,#863),#1148,.F.);
#8621=ADVANCED_FACE('',(#1596),#8200,.F.);
#8622=ADVANCED_FACE('',(#1597),#8201,.T.);
#8623=ADVANCED_FACE('',(#1598,#864),#1149,.T.);
#8624=ADVANCED_FACE('',(#1599,#865),#1150,.F.);
#8625=ADVANCED_FACE('',(#1600),#8202,.F.);
#8626=ADVANCED_FACE('',(#1601),#8203,.F.);
#8627=ADVANCED_FACE('',(#1602),#8204,.T.);
#8628=ADVANCED_FACE('',(#1603),#1151,.T.);
#8629=ADVANCED_FACE('',(#1604,#866,#867),#1152,.F.);
#8630=ADVANCED_FACE('',(#1605),#1153,.T.);
#8631=ADVANCED_FACE('',(#1606),#8205,.T.);
#8632=ADVANCED_FACE('',(#1607,#868,#869),#1154,.T.);
#8633=ADVANCED_FACE('',(#1608),#8206,.F.);
#8634=ADVANCED_FACE('',(#1609),#8207,.T.);
#8635=ADVANCED_FACE('',(#1610,#870),#1155,.T.);
#8636=ADVANCED_FACE('',(#1611,#871),#1156,.F.);
#8637=ADVANCED_FACE('',(#1612),#8208,.F.);
#8638=ADVANCED_FACE('',(#1613),#8209,.T.);
#8639=ADVANCED_FACE('',(#1614,#872),#1157,.T.);
#8640=ADVANCED_FACE('',(#1615,#873),#1158,.F.);
#8641=ADVANCED_FACE('',(#1616),#8210,.F.);
#8642=ADVANCED_FACE('',(#1617),#1159,.T.);
#8643=ADVANCED_FACE('',(#1618),#8211,.F.);
#8644=ADVANCED_FACE('',(#1619),#8212,.F.);
#8645=ADVANCED_FACE('',(#1620),#8213,.F.);
#8646=ADVANCED_FACE('',(#1621),#8214,.F.);
#8647=ADVANCED_FACE('',(#1622),#8215,.F.);
#8648=ADVANCED_FACE('',(#1623),#1160,.T.);
#8649=ADVANCED_FACE('',(#1624,#874,#875,#876,#877,#878),#1161,.T.);
#8650=ADVANCED_FACE('',(#1625),#1162,.T.);
#8651=ADVANCED_FACE('',(#1626,#879,#880,#881,#882,#883),#1163,.T.);
#8652=ADVANCED_FACE('',(#1627,#884),#1164,.T.);
#8653=ADVANCED_FACE('',(#1628),#1165,.F.);
#8654=ADVANCED_FACE('',(#1629),#8216,.F.);
#8655=ADVANCED_FACE('',(#1630),#8217,.F.);
#8656=ADVANCED_FACE('',(#1631),#8218,.F.);
#8657=ADVANCED_FACE('',(#1632),#8219,.F.);
#8658=ADVANCED_FACE('',(#1633),#8220,.F.);
#8659=ADVANCED_FACE('',(#1634),#1166,.T.);
#8660=ADVANCED_FACE('',(#1635,#885,#886,#887,#888,#889),#1167,.T.);
#8661=ADVANCED_FACE('',(#1636),#1168,.T.);
#8662=ADVANCED_FACE('',(#1637,#890,#891,#892,#893,#894),#1169,.T.);
#8663=ADVANCED_FACE('',(#1638),#1170,.T.);
#8664=ADVANCED_FACE('',(#1639),#1171,.F.);
#8665=ADVANCED_FACE('',(#1640),#8221,.F.);
#8666=ADVANCED_FACE('',(#1641),#8222,.F.);
#8667=ADVANCED_FACE('',(#1642),#8223,.F.);
#8668=ADVANCED_FACE('',(#1643),#8224,.F.);
#8669=ADVANCED_FACE('',(#1644),#8225,.F.);
#8670=ADVANCED_FACE('',(#1645),#1172,.T.);
#8671=ADVANCED_FACE('',(#1646,#895,#896,#897,#898,#899),#1173,.T.);
#8672=ADVANCED_FACE('',(#1647),#1174,.T.);
#8673=ADVANCED_FACE('',(#1648,#900,#901,#902,#903,#904),#1175,.T.);
#8674=ADVANCED_FACE('',(#1649),#1176,.T.);
#8675=ADVANCED_FACE('',(#1650),#1177,.F.);
#8676=ADVANCED_FACE('',(#1651),#8226,.F.);
#8677=ADVANCED_FACE('',(#1652),#1178,.T.);
#8678=ADVANCED_FACE('',(#1653,#905),#1179,.T.);
#8679=ADVANCED_FACE('',(#1654,#906),#1180,.F.);
#8680=ADVANCED_FACE('',(#1655),#8227,.T.);
#8681=ADVANCED_FACE('',(#1656),#8228,.T.);
#8682=ADVANCED_FACE('',(#1657),#8229,.T.);
#8683=ADVANCED_FACE('',(#1658,#907),#1181,.T.);
#8684=ADVANCED_FACE('',(#1659),#1182,.F.);
#8685=ADVANCED_FACE('',(#1660),#8230,.F.);
#8686=ADVANCED_FACE('',(#1661),#8231,.T.);
#8687=ADVANCED_FACE('',(#1662,#908),#1183,.T.);
#8688=ADVANCED_FACE('',(#1663,#909),#1184,.F.);
#8689=ADVANCED_FACE('',(#1664),#8232,.F.);
#8690=ADVANCED_FACE('',(#1665),#8233,.T.);
#8691=ADVANCED_FACE('',(#1666,#910),#1185,.T.);
#8692=ADVANCED_FACE('',(#1667,#911),#1186,.F.);
#8693=ADVANCED_FACE('',(#1668),#8234,.F.);
#8694=ADVANCED_FACE('',(#1669),#8235,.T.);
#8695=ADVANCED_FACE('',(#1670,#912),#1187,.T.);
#8696=ADVANCED_FACE('',(#1671,#913),#1188,.F.);
#8697=ADVANCED_FACE('',(#1672),#8236,.F.);
#8698=ADVANCED_FACE('',(#1673),#1189,.T.);
#8699=ADVANCED_FACE('',(#1674),#8237,.F.);
#8700=ADVANCED_FACE('',(#1675),#8238,.F.);
#8701=ADVANCED_FACE('',(#1676),#8239,.F.);
#8702=ADVANCED_FACE('',(#1677),#8240,.F.);
#8703=ADVANCED_FACE('',(#1678),#8241,.F.);
#8704=ADVANCED_FACE('',(#1679,#914,#915,#916,#917,#918),#1190,.T.);
#8705=ADVANCED_FACE('',(#1680),#1191,.T.);
#8706=ADVANCED_FACE('',(#1681,#919,#920,#921,#922,#923),#1192,.T.);
#8707=ADVANCED_FACE('',(#1682),#1193,.T.);
#8708=ADVANCED_FACE('',(#1683,#924),#1194,.T.);
#8709=ADVANCED_FACE('',(#1684),#1195,.F.);
#8710=ADVANCED_FACE('',(#1685),#8242,.F.);
#8711=ADVANCED_FACE('',(#1686),#8243,.F.);
#8712=ADVANCED_FACE('',(#1687),#8244,.F.);
#8713=ADVANCED_FACE('',(#1688),#8245,.F.);
#8714=ADVANCED_FACE('',(#1689),#8246,.F.);
#8715=ADVANCED_FACE('',(#1690,#925,#926,#927,#928,#929),#1196,.T.);
#8716=ADVANCED_FACE('',(#1691),#1197,.T.);
#8717=ADVANCED_FACE('',(#1692,#930,#931,#932,#933,#934),#1198,.T.);
#8718=ADVANCED_FACE('',(#1693),#1199,.T.);
#8719=ADVANCED_FACE('',(#1694),#1200,.T.);
#8720=ADVANCED_FACE('',(#1695),#1201,.F.);
#8721=ADVANCED_FACE('',(#1696),#8247,.F.);
#8722=ADVANCED_FACE('',(#1697),#8248,.F.);
#8723=ADVANCED_FACE('',(#1698),#8249,.F.);
#8724=ADVANCED_FACE('',(#1699),#8250,.F.);
#8725=ADVANCED_FACE('',(#1700),#8251,.F.);
#8726=ADVANCED_FACE('',(#1701,#935,#936,#937,#938,#939),#1202,.T.);
#8727=ADVANCED_FACE('',(#1702),#1203,.T.);
#8728=ADVANCED_FACE('',(#1703,#940,#941,#942,#943,#944),#1204,.T.);
#8729=ADVANCED_FACE('',(#1704),#1205,.T.);
#8730=ADVANCED_FACE('',(#1705),#1206,.T.);
#8731=ADVANCED_FACE('',(#1706),#1207,.F.);
#8732=ADVANCED_FACE('',(#1707),#8252,.F.);
#8733=ADVANCED_FACE('',(#1708),#1208,.T.);
#8734=ADVANCED_FACE('',(#1709,#945),#1209,.T.);
#8735=ADVANCED_FACE('',(#1710,#946),#1210,.F.);
#8736=ADVANCED_FACE('',(#1711),#8253,.T.);
#8737=ADVANCED_FACE('',(#1712),#8254,.T.);
#8738=ADVANCED_FACE('',(#1713),#8255,.T.);
#8739=ADVANCED_FACE('',(#1714,#947),#1211,.T.);
#8740=ADVANCED_FACE('',(#1715),#1212,.F.);
#8741=ADVANCED_FACE('',(#1716),#8256,.F.);
#8742=ADVANCED_FACE('',(#1717),#8257,.T.);
#8743=ADVANCED_FACE('',(#1718,#948),#1213,.T.);
#8744=ADVANCED_FACE('',(#1719,#949),#1214,.F.);
#8745=ADVANCED_FACE('',(#1720),#8258,.F.);
#8746=ADVANCED_FACE('',(#1721),#8259,.T.);
#8747=ADVANCED_FACE('',(#1722,#950),#1215,.T.);
#8748=ADVANCED_FACE('',(#1723,#951),#1216,.F.);
#8749=ADVANCED_FACE('',(#1724),#8260,.F.);
#8750=ADVANCED_FACE('',(#1725),#8261,.T.);
#8751=ADVANCED_FACE('',(#1726,#952),#1217,.T.);
#8752=ADVANCED_FACE('',(#1727,#953),#1218,.F.);
#8753=ADVANCED_FACE('',(#1728),#1219,.F.);
#8754=ADVANCED_FACE('',(#1729),#1220,.F.);
#8755=ADVANCED_FACE('',(#1730),#1221,.F.);
#8756=ADVANCED_FACE('',(#1731),#1222,.F.);
#8757=ADVANCED_FACE('',(#1732),#1223,.F.);
#8758=ADVANCED_FACE('',(#1733,#954),#1224,.T.);
#8759=ADVANCED_FACE('',(#1734),#8262,.T.);
#8760=ADVANCED_FACE('',(#1735,#955),#1225,.T.);
#8761=ADVANCED_FACE('',(#1736),#8263,.T.);
#8762=ADVANCED_FACE('',(#1737,#956),#1226,.T.);
#8763=ADVANCED_FACE('',(#1738),#8264,.T.);
#8764=ADVANCED_FACE('',(#1739,#957),#1227,.T.);
#8765=ADVANCED_FACE('',(#1740),#8265,.T.);
#8766=ADVANCED_FACE('',(#1741,#958),#1228,.T.);
#8767=ADVANCED_FACE('',(#1742),#8266,.T.);
#8768=ADVANCED_FACE('',(#1743,#959),#1229,.T.);
#8769=ADVANCED_FACE('',(#1744,#960),#8267,.F.);
#8770=ADVANCED_FACE('',(#1745),#1230,.F.);
#8771=ADVANCED_FACE('',(#1746),#1231,.F.);
#8772=ADVANCED_FACE('',(#1747),#1232,.F.);
#8773=ADVANCED_FACE('',(#1748),#1233,.F.);
#8774=ADVANCED_FACE('',(#1749,#961),#1234,.T.);
#8775=ADVANCED_FACE('',(#1750,#962),#8268,.T.);
#8776=ADVANCED_FACE('',(#1751,#963),#1235,.T.);
#8777=ADVANCED_FACE('',(#1752,#964),#8269,.F.);
#8778=ADVANCED_FACE('',(#1753),#1236,.F.);
#8779=ADVANCED_FACE('',(#1754),#1237,.F.);
#8780=ADVANCED_FACE('',(#1755),#1238,.F.);
#8781=ADVANCED_FACE('',(#1756),#1239,.F.);
#8782=ADVANCED_FACE('',(#1757),#1240,.F.);
#8783=ADVANCED_FACE('',(#1758),#1241,.F.);
#8784=ADVANCED_FACE('',(#1759),#1242,.F.);
#8785=ADVANCED_FACE('',(#1760),#1243,.F.);
#8786=ADVANCED_FACE('',(#1761),#1244,.F.);
#8787=ADVANCED_FACE('',(#1762),#1245,.T.);
#8788=ADVANCED_FACE('',(#1763),#448,.T.);
#8789=ADVANCED_FACE('',(#1764),#8270,.T.);
#8790=ADVANCED_FACE('',(#1765),#449,.T.);
#8791=ADVANCED_FACE('',(#1766,#965),#1246,.T.);
#8792=ADVANCED_FACE('',(#1767),#450,.T.);
#8793=ADVANCED_FACE('',(#1768),#8271,.T.);
#8794=CLOSED_SHELL('',(#8272,#8273,#8274,#8275,#8276,#8277,#8278,#8279,
#8280,#8281,#8282,#8283,#8284,#8285,#8286,#8287,#8288,#8289));
#8795=CLOSED_SHELL('',(#8290,#8291,#8292,#8293,#8294,#8295));
#8796=CLOSED_SHELL('',(#8296,#8297,#8298,#8299,#8300,#8301));
#8797=CLOSED_SHELL('',(#8302,#8303,#8304,#8305,#8306,#8307,#8308,#8309,
#8310,#8311,#8312,#8313,#8314,#8315,#8316,#8317,#8318,#8319,#8320,#8321,
#8322,#8323,#8324,#8325,#8326,#8327,#8328,#8329,#8330));
#8798=CLOSED_SHELL('',(#8331,#8332,#8333,#8334,#8335,#8336,#8337,#8338,
#8339,#8340,#8341,#8342,#8343,#8344,#8345,#8346,#8347,#8348));
#8799=CLOSED_SHELL('',(#8349,#8350,#8351,#8352,#8353,#8354,#8355,#8356,
#8357,#8358,#8359,#8360,#8361,#8362,#8363,#8364,#8365,#8366));
#8800=CLOSED_SHELL('',(#8367,#8368,#8369,#8370,#8371,#8372,#8373,#8374,
#8375,#8376,#8377,#8378,#8379,#8380,#8381,#8382,#8383,#8384));
#8801=CLOSED_SHELL('',(#8385,#8386,#8387,#8388,#8389,#8390,#8391,#8392,
#8393,#8394,#8395,#8396,#8397,#8398,#8399,#8400,#8401));
#8802=CLOSED_SHELL('',(#8402,#8403,#8404,#8405,#8406,#8407,#8408,#8409,
#8410,#8411,#8412,#8413,#8414,#8415,#8416,#8417,#8418));
#8803=CLOSED_SHELL('',(#8419,#8420,#8421,#8422,#8423,#8424,#8425,#8426));
#8804=CLOSED_SHELL('',(#8427,#8428,#8429,#8430,#8431,#8432,#8433,#8434));
#8805=CLOSED_SHELL('',(#8435,#8436,#8437,#8438,#8439,#8440,#8441,#8442));
#8806=CLOSED_SHELL('',(#8443,#8444,#8445,#8446,#8447,#8448,#8449,#8450));
#8807=CLOSED_SHELL('',(#8451));
#8808=CLOSED_SHELL('',(#8452));
#8809=CLOSED_SHELL('',(#8453));
#8810=CLOSED_SHELL('',(#8454));
#8811=CLOSED_SHELL('',(#8455));
#8812=CLOSED_SHELL('',(#8456));
#8813=CLOSED_SHELL('',(#8457));
#8814=CLOSED_SHELL('',(#8458));
#8815=CLOSED_SHELL('',(#8459,#8460,#8461,#8462,#8463,#8464,#8465,#8466,
#8467,#8468,#8469,#8470,#8471,#8472,#8473,#8474,#8475,#8476,#8477));
#8816=CLOSED_SHELL('',(#8478,#8479,#8480,#8481));
#8817=CLOSED_SHELL('',(#8482,#8483,#8484,#8485));
#8818=CLOSED_SHELL('',(#8486,#8487,#8488,#8489));
#8819=CLOSED_SHELL('',(#8490,#8491,#8492,#8493,#8494,#8495,#8496,#8497,
#8498,#8499,#8500,#8501));
#8820=CLOSED_SHELL('',(#8502,#8503,#8504,#8505,#8506,#8507,#8508,#8509,
#8510,#8511,#8512,#8513,#8514,#8515,#8516,#8517,#8518,#8519,#8520,#8521,
#8522));
#8821=CLOSED_SHELL('',(#8523,#8524,#8525,#8526,#8527));
#8822=CLOSED_SHELL('',(#8528,#8529,#8530,#8531));
#8823=CLOSED_SHELL('',(#8532,#8533,#8534,#8535,#8536,#8537,#8538));
#8824=CLOSED_SHELL('',(#8539,#8540,#8541,#8542,#8543,#8544,#8545,#8546,
#8547));
#8825=CLOSED_SHELL('',(#8548,#8549,#8550,#8551));
#8826=CLOSED_SHELL('',(#8552,#8553,#8554,#8555));
#8827=CLOSED_SHELL('',(#8556,#8557,#8558,#8559));
#8828=CLOSED_SHELL('',(#8560,#8561,#8562,#8563,#8564,#8565,#8566,#8567,
#8568));
#8829=CLOSED_SHELL('',(#8569,#8570,#8571,#8572));
#8830=CLOSED_SHELL('',(#8573,#8574,#8575,#8576));
#8831=CLOSED_SHELL('',(#8577,#8578,#8579,#8580));
#8832=CLOSED_SHELL('',(#8581,#8582,#8583,#8584,#8585,#8586,#8587,#8588,
#8589));
#8833=CLOSED_SHELL('',(#8590,#8591,#8592,#8593,#8594,#8595,#8596,#8597));
#8834=CLOSED_SHELL('',(#8598,#8599,#8600,#8601,#8602,#8603,#8604,#8605,
#8606,#8607,#8608));
#8835=CLOSED_SHELL('',(#8609,#8610,#8611,#8612,#8613,#8614,#8615,#8616));
#8836=CLOSED_SHELL('',(#8617,#8618,#8619,#8620));
#8837=CLOSED_SHELL('',(#8621,#8622,#8623,#8624));
#8838=CLOSED_SHELL('',(#8625,#8626,#8627,#8628,#8629,#8630,#8631,#8632));
#8839=CLOSED_SHELL('',(#8633,#8634,#8635,#8636));
#8840=CLOSED_SHELL('',(#8637,#8638,#8639,#8640));
#8841=CLOSED_SHELL('',(#8641,#8642,#8643,#8644,#8645,#8646,#8647,#8648,
#8649,#8650,#8651,#8652,#8653));
#8842=CLOSED_SHELL('',(#8654,#8655,#8656,#8657,#8658,#8659,#8660,#8661,
#8662,#8663,#8664));
#8843=CLOSED_SHELL('',(#8665,#8666,#8667,#8668,#8669,#8670,#8671,#8672,
#8673,#8674,#8675));
#8844=CLOSED_SHELL('',(#8676,#8677,#8678,#8679,#8680,#8681,#8682,#8683,
#8684));
#8845=CLOSED_SHELL('',(#8685,#8686,#8687,#8688));
#8846=CLOSED_SHELL('',(#8689,#8690,#8691,#8692));
#8847=CLOSED_SHELL('',(#8693,#8694,#8695,#8696));
#8848=CLOSED_SHELL('',(#8697,#8698,#8699,#8700,#8701,#8702,#8703,#8704,
#8705,#8706,#8707,#8708,#8709));
#8849=CLOSED_SHELL('',(#8710,#8711,#8712,#8713,#8714,#8715,#8716,#8717,
#8718,#8719,#8720));
#8850=CLOSED_SHELL('',(#8721,#8722,#8723,#8724,#8725,#8726,#8727,#8728,
#8729,#8730,#8731));
#8851=CLOSED_SHELL('',(#8732,#8733,#8734,#8735,#8736,#8737,#8738,#8739,
#8740));
#8852=CLOSED_SHELL('',(#8741,#8742,#8743,#8744));
#8853=CLOSED_SHELL('',(#8745,#8746,#8747,#8748));
#8854=CLOSED_SHELL('',(#8749,#8750,#8751,#8752));
#8855=CLOSED_SHELL('',(#8753,#8754,#8755,#8756,#8757,#8758,#8759,#8760,
#8761,#8762,#8763,#8764,#8765,#8766,#8767,#8768,#8769));
#8856=CLOSED_SHELL('',(#8770,#8771,#8772,#8773,#8774,#8775,#8776,#8777));
#8857=CLOSED_SHELL('',(#8778,#8779,#8780,#8781,#8782,#8783,#8784,#8785));
#8858=CLOSED_SHELL('',(#8786,#8787,#8788,#8789,#8790,#8791,#8792,#8793));
#8859=DERIVED_UNIT_ELEMENT(#8967,1.);
#8860=DERIVED_UNIT_ELEMENT(#16680,-3.);
#8861=DERIVED_UNIT_ELEMENT(#8967,1.);
#8862=DERIVED_UNIT_ELEMENT(#16680,-3.);
#8863=DERIVED_UNIT_ELEMENT(#8967,1.);
#8864=DERIVED_UNIT_ELEMENT(#16680,-3.);
#8865=DERIVED_UNIT_ELEMENT(#8967,1.);
#8866=DERIVED_UNIT_ELEMENT(#16680,-3.);
#8867=DERIVED_UNIT_ELEMENT(#8967,1.);
#8868=DERIVED_UNIT_ELEMENT(#16680,-3.);
#8869=DERIVED_UNIT_ELEMENT(#8967,1.);
#8870=DERIVED_UNIT_ELEMENT(#16680,-3.);
#8871=DERIVED_UNIT_ELEMENT(#8967,1.);
#8872=DERIVED_UNIT_ELEMENT(#16680,-3.);
#8873=DERIVED_UNIT_ELEMENT(#8967,1.);
#8874=DERIVED_UNIT_ELEMENT(#16680,-3.);
#8875=DERIVED_UNIT_ELEMENT(#8967,1.);
#8876=DERIVED_UNIT_ELEMENT(#16680,-3.);
#8877=DERIVED_UNIT_ELEMENT(#8967,1.);
#8878=DERIVED_UNIT_ELEMENT(#16680,-3.);
#8879=DERIVED_UNIT_ELEMENT(#8967,1.);
#8880=DERIVED_UNIT_ELEMENT(#16680,-3.);
#8881=DERIVED_UNIT_ELEMENT(#8967,1.);
#8882=DERIVED_UNIT_ELEMENT(#16680,-3.);
#8883=DERIVED_UNIT_ELEMENT(#8967,1.);
#8884=DERIVED_UNIT_ELEMENT(#16680,-3.);
#8885=DERIVED_UNIT_ELEMENT(#8967,1.);
#8886=DERIVED_UNIT_ELEMENT(#16680,-3.);
#8887=DERIVED_UNIT_ELEMENT(#8967,1.);
#8888=DERIVED_UNIT_ELEMENT(#16680,-3.);
#8889=DERIVED_UNIT_ELEMENT(#8967,1.);
#8890=DERIVED_UNIT_ELEMENT(#16680,-3.);
#8891=DERIVED_UNIT_ELEMENT(#8967,1.);
#8892=DERIVED_UNIT_ELEMENT(#16680,-3.);
#8893=DERIVED_UNIT_ELEMENT(#8967,1.);
#8894=DERIVED_UNIT_ELEMENT(#16680,-3.);
#8895=DERIVED_UNIT_ELEMENT(#8967,1.);
#8896=DERIVED_UNIT_ELEMENT(#16680,-3.);
#8897=DERIVED_UNIT_ELEMENT(#8967,1.);
#8898=DERIVED_UNIT_ELEMENT(#16680,-3.);
#8899=DERIVED_UNIT_ELEMENT(#8967,1.);
#8900=DERIVED_UNIT_ELEMENT(#16680,-3.);
#8901=DERIVED_UNIT_ELEMENT(#8967,1.);
#8902=DERIVED_UNIT_ELEMENT(#16680,-3.);
#8903=DERIVED_UNIT_ELEMENT(#8967,1.);
#8904=DERIVED_UNIT_ELEMENT(#16680,-3.);
#8905=DERIVED_UNIT_ELEMENT(#8967,1.);
#8906=DERIVED_UNIT_ELEMENT(#16680,-3.);
#8907=DERIVED_UNIT_ELEMENT(#8967,1.);
#8908=DERIVED_UNIT_ELEMENT(#16680,-3.);
#8909=DERIVED_UNIT_ELEMENT(#8967,1.);
#8910=DERIVED_UNIT_ELEMENT(#16680,-3.);
#8911=DERIVED_UNIT_ELEMENT(#8967,1.);
#8912=DERIVED_UNIT_ELEMENT(#16680,-3.);
#8913=DERIVED_UNIT_ELEMENT(#8967,1.);
#8914=DERIVED_UNIT_ELEMENT(#16680,-3.);
#8915=DERIVED_UNIT_ELEMENT(#8967,1.);
#8916=DERIVED_UNIT_ELEMENT(#16680,-3.);
#8917=DERIVED_UNIT_ELEMENT(#8967,1.);
#8918=DERIVED_UNIT_ELEMENT(#16680,-3.);
#8919=DERIVED_UNIT_ELEMENT(#8967,1.);
#8920=DERIVED_UNIT_ELEMENT(#16680,-3.);
#8921=DERIVED_UNIT_ELEMENT(#8967,1.);
#8922=DERIVED_UNIT_ELEMENT(#16680,-3.);
#8923=DERIVED_UNIT_ELEMENT(#8967,1.);
#8924=DERIVED_UNIT_ELEMENT(#16680,-3.);
#8925=DERIVED_UNIT_ELEMENT(#8967,1.);
#8926=DERIVED_UNIT_ELEMENT(#16680,-3.);
#8927=DERIVED_UNIT_ELEMENT(#8967,1.);
#8928=DERIVED_UNIT_ELEMENT(#16680,-3.);
#8929=DERIVED_UNIT_ELEMENT(#8967,1.);
#8930=DERIVED_UNIT_ELEMENT(#16680,-3.);
#8931=DERIVED_UNIT_ELEMENT(#8967,1.);
#8932=DERIVED_UNIT_ELEMENT(#16680,-3.);
#8933=DERIVED_UNIT_ELEMENT(#8967,1.);
#8934=DERIVED_UNIT_ELEMENT(#16680,-3.);
#8935=DERIVED_UNIT_ELEMENT(#8967,1.);
#8936=DERIVED_UNIT_ELEMENT(#16680,-3.);
#8937=DERIVED_UNIT_ELEMENT(#8967,1.);
#8938=DERIVED_UNIT_ELEMENT(#16680,-3.);
#8939=DERIVED_UNIT_ELEMENT(#8967,1.);
#8940=DERIVED_UNIT_ELEMENT(#16680,-3.);
#8941=DERIVED_UNIT_ELEMENT(#8967,1.);
#8942=DERIVED_UNIT_ELEMENT(#16680,-3.);
#8943=DERIVED_UNIT_ELEMENT(#8967,1.);
#8944=DERIVED_UNIT_ELEMENT(#16680,-3.);
#8945=DERIVED_UNIT_ELEMENT(#8967,1.);
#8946=DERIVED_UNIT_ELEMENT(#16680,-3.);
#8947=DERIVED_UNIT_ELEMENT(#8967,1.);
#8948=DERIVED_UNIT_ELEMENT(#16680,-3.);
#8949=DERIVED_UNIT_ELEMENT(#8967,1.);
#8950=DERIVED_UNIT_ELEMENT(#16680,-3.);
#8951=DERIVED_UNIT_ELEMENT(#8967,1.);
#8952=DERIVED_UNIT_ELEMENT(#16680,-3.);
#8953=DERIVED_UNIT_ELEMENT(#8967,1.);
#8954=DERIVED_UNIT_ELEMENT(#16680,-3.);
#8955=DERIVED_UNIT_ELEMENT(#8967,1.);
#8956=DERIVED_UNIT_ELEMENT(#16680,-3.);
#8957=DERIVED_UNIT_ELEMENT(#8967,1.);
#8958=DERIVED_UNIT_ELEMENT(#16680,-3.);
#8959=DERIVED_UNIT_ELEMENT(#8967,1.);
#8960=DERIVED_UNIT_ELEMENT(#16680,-3.);
#8961=DERIVED_UNIT_ELEMENT(#8967,1.);
#8962=DERIVED_UNIT_ELEMENT(#16680,-3.);
#8963=DERIVED_UNIT_ELEMENT(#8967,1.);
#8964=DERIVED_UNIT_ELEMENT(#16680,-3.);
#8965=DERIVED_UNIT_ELEMENT(#8967,1.);
#8966=DERIVED_UNIT_ELEMENT(#16680,-3.);
#8967=(
MASS_UNIT()
NAMED_UNIT(*)
SI_UNIT(.KILO.,.GRAM.)
);
#8968=DERIVED_UNIT((#8859,#8860));
#8969=DERIVED_UNIT((#8861,#8862));
#8970=DERIVED_UNIT((#8863,#8864));
#8971=DERIVED_UNIT((#8865,#8866));
#8972=DERIVED_UNIT((#8867,#8868));
#8973=DERIVED_UNIT((#8869,#8870));
#8974=DERIVED_UNIT((#8871,#8872));
#8975=DERIVED_UNIT((#8873,#8874));
#8976=DERIVED_UNIT((#8875,#8876));
#8977=DERIVED_UNIT((#8877,#8878));
#8978=DERIVED_UNIT((#8879,#8880));
#8979=DERIVED_UNIT((#8881,#8882));
#8980=DERIVED_UNIT((#8883,#8884));
#8981=DERIVED_UNIT((#8885,#8886));
#8982=DERIVED_UNIT((#8887,#8888));
#8983=DERIVED_UNIT((#8889,#8890));
#8984=DERIVED_UNIT((#8891,#8892));
#8985=DERIVED_UNIT((#8893,#8894));
#8986=DERIVED_UNIT((#8895,#8896));
#8987=DERIVED_UNIT((#8897,#8898));
#8988=DERIVED_UNIT((#8899,#8900));
#8989=DERIVED_UNIT((#8901,#8902));
#8990=DERIVED_UNIT((#8903,#8904));
#8991=DERIVED_UNIT((#8905,#8906));
#8992=DERIVED_UNIT((#8907,#8908));
#8993=DERIVED_UNIT((#8909,#8910));
#8994=DERIVED_UNIT((#8911,#8912));
#8995=DERIVED_UNIT((#8913,#8914));
#8996=DERIVED_UNIT((#8915,#8916));
#8997=DERIVED_UNIT((#8917,#8918));
#8998=DERIVED_UNIT((#8919,#8920));
#8999=DERIVED_UNIT((#8921,#8922));
#9000=DERIVED_UNIT((#8923,#8924));
#9001=DERIVED_UNIT((#8925,#8926));
#9002=DERIVED_UNIT((#8927,#8928));
#9003=DERIVED_UNIT((#8929,#8930));
#9004=DERIVED_UNIT((#8931,#8932));
#9005=DERIVED_UNIT((#8933,#8934));
#9006=DERIVED_UNIT((#8935,#8936));
#9007=DERIVED_UNIT((#8937,#8938));
#9008=DERIVED_UNIT((#8939,#8940));
#9009=DERIVED_UNIT((#8941,#8942));
#9010=DERIVED_UNIT((#8943,#8944));
#9011=DERIVED_UNIT((#8945,#8946));
#9012=DERIVED_UNIT((#8947,#8948));
#9013=DERIVED_UNIT((#8949,#8950));
#9014=DERIVED_UNIT((#8951,#8952));
#9015=DERIVED_UNIT((#8953,#8954));
#9016=DERIVED_UNIT((#8955,#8956));
#9017=DERIVED_UNIT((#8957,#8958));
#9018=DERIVED_UNIT((#8959,#8960));
#9019=DERIVED_UNIT((#8961,#8962));
#9020=DERIVED_UNIT((#8963,#8964));
#9021=DERIVED_UNIT((#8965,#8966));
#9022=MEASURE_REPRESENTATION_ITEM('density measure',
POSITIVE_RATIO_MEASURE(7850.),#8968);
#9023=MEASURE_REPRESENTATION_ITEM('density measure',
POSITIVE_RATIO_MEASURE(7850.),#8969);
#9024=MEASURE_REPRESENTATION_ITEM('density measure',
POSITIVE_RATIO_MEASURE(7850.),#8970);
#9025=MEASURE_REPRESENTATION_ITEM('density measure',
POSITIVE_RATIO_MEASURE(7850.),#8971);
#9026=MEASURE_REPRESENTATION_ITEM('density measure',
POSITIVE_RATIO_MEASURE(7850.),#8972);
#9027=MEASURE_REPRESENTATION_ITEM('density measure',
POSITIVE_RATIO_MEASURE(7850.),#8973);
#9028=MEASURE_REPRESENTATION_ITEM('density measure',
POSITIVE_RATIO_MEASURE(7850.),#8974);
#9029=MEASURE_REPRESENTATION_ITEM('density measure',
POSITIVE_RATIO_MEASURE(7850.),#8975);
#9030=MEASURE_REPRESENTATION_ITEM('density measure',
POSITIVE_RATIO_MEASURE(7850.),#8976);
#9031=MEASURE_REPRESENTATION_ITEM('density measure',
POSITIVE_RATIO_MEASURE(7850.),#8977);
#9032=MEASURE_REPRESENTATION_ITEM('density measure',
POSITIVE_RATIO_MEASURE(7850.),#8978);
#9033=MEASURE_REPRESENTATION_ITEM('density measure',
POSITIVE_RATIO_MEASURE(7850.),#8979);
#9034=MEASURE_REPRESENTATION_ITEM('density measure',
POSITIVE_RATIO_MEASURE(7850.),#8980);
#9035=MEASURE_REPRESENTATION_ITEM('density measure',
POSITIVE_RATIO_MEASURE(7850.),#8981);
#9036=MEASURE_REPRESENTATION_ITEM('density measure',
POSITIVE_RATIO_MEASURE(7850.),#8982);
#9037=MEASURE_REPRESENTATION_ITEM('density measure',
POSITIVE_RATIO_MEASURE(7850.),#8983);
#9038=MEASURE_REPRESENTATION_ITEM('density measure',
POSITIVE_RATIO_MEASURE(7850.),#8984);
#9039=MEASURE_REPRESENTATION_ITEM('density measure',
POSITIVE_RATIO_MEASURE(7850.),#8985);
#9040=MEASURE_REPRESENTATION_ITEM('density measure',
POSITIVE_RATIO_MEASURE(7850.),#8986);
#9041=MEASURE_REPRESENTATION_ITEM('density measure',
POSITIVE_RATIO_MEASURE(7850.),#8987);
#9042=MEASURE_REPRESENTATION_ITEM('density measure',
POSITIVE_RATIO_MEASURE(7850.),#8988);
#9043=MEASURE_REPRESENTATION_ITEM('density measure',
POSITIVE_RATIO_MEASURE(7850.),#8989);
#9044=MEASURE_REPRESENTATION_ITEM('density measure',
POSITIVE_RATIO_MEASURE(7850.),#8990);
#9045=MEASURE_REPRESENTATION_ITEM('density measure',
POSITIVE_RATIO_MEASURE(7850.),#8991);
#9046=MEASURE_REPRESENTATION_ITEM('density measure',
POSITIVE_RATIO_MEASURE(7850.),#8992);
#9047=MEASURE_REPRESENTATION_ITEM('density measure',
POSITIVE_RATIO_MEASURE(7850.),#8993);
#9048=MEASURE_REPRESENTATION_ITEM('density measure',
POSITIVE_RATIO_MEASURE(7850.),#8994);
#9049=MEASURE_REPRESENTATION_ITEM('density measure',
POSITIVE_RATIO_MEASURE(7850.),#8995);
#9050=MEASURE_REPRESENTATION_ITEM('density measure',
POSITIVE_RATIO_MEASURE(7850.),#8996);
#9051=MEASURE_REPRESENTATION_ITEM('density measure',
POSITIVE_RATIO_MEASURE(7850.),#8997);
#9052=MEASURE_REPRESENTATION_ITEM('density measure',
POSITIVE_RATIO_MEASURE(7850.),#8998);
#9053=MEASURE_REPRESENTATION_ITEM('density measure',
POSITIVE_RATIO_MEASURE(7850.),#8999);
#9054=MEASURE_REPRESENTATION_ITEM('density measure',
POSITIVE_RATIO_MEASURE(7850.),#9000);
#9055=MEASURE_REPRESENTATION_ITEM('density measure',
POSITIVE_RATIO_MEASURE(7850.),#9001);
#9056=MEASURE_REPRESENTATION_ITEM('density measure',
POSITIVE_RATIO_MEASURE(7850.),#9002);
#9057=MEASURE_REPRESENTATION_ITEM('density measure',
POSITIVE_RATIO_MEASURE(7850.),#9003);
#9058=MEASURE_REPRESENTATION_ITEM('density measure',
POSITIVE_RATIO_MEASURE(7850.),#9004);
#9059=MEASURE_REPRESENTATION_ITEM('density measure',
POSITIVE_RATIO_MEASURE(7850.),#9005);
#9060=MEASURE_REPRESENTATION_ITEM('density measure',
POSITIVE_RATIO_MEASURE(7850.),#9006);
#9061=MEASURE_REPRESENTATION_ITEM('density measure',
POSITIVE_RATIO_MEASURE(7850.),#9007);
#9062=MEASURE_REPRESENTATION_ITEM('density measure',
POSITIVE_RATIO_MEASURE(7850.),#9008);
#9063=MEASURE_REPRESENTATION_ITEM('density measure',
POSITIVE_RATIO_MEASURE(7850.),#9009);
#9064=MEASURE_REPRESENTATION_ITEM('density measure',
POSITIVE_RATIO_MEASURE(7850.),#9010);
#9065=MEASURE_REPRESENTATION_ITEM('density measure',
POSITIVE_RATIO_MEASURE(7850.),#9011);
#9066=MEASURE_REPRESENTATION_ITEM('density measure',
POSITIVE_RATIO_MEASURE(7850.),#9012);
#9067=MEASURE_REPRESENTATION_ITEM('density measure',
POSITIVE_RATIO_MEASURE(7850.),#9013);
#9068=MEASURE_REPRESENTATION_ITEM('density measure',
POSITIVE_RATIO_MEASURE(7850.),#9014);
#9069=MEASURE_REPRESENTATION_ITEM('density measure',
POSITIVE_RATIO_MEASURE(7850.),#9015);
#9070=MEASURE_REPRESENTATION_ITEM('density measure',
POSITIVE_RATIO_MEASURE(7850.),#9016);
#9071=MEASURE_REPRESENTATION_ITEM('density measure',
POSITIVE_RATIO_MEASURE(7850.),#9017);
#9072=MEASURE_REPRESENTATION_ITEM('density measure',
POSITIVE_RATIO_MEASURE(7850.),#9018);
#9073=MEASURE_REPRESENTATION_ITEM('density measure',
POSITIVE_RATIO_MEASURE(7850.),#9019);
#9074=MEASURE_REPRESENTATION_ITEM('density measure',
POSITIVE_RATIO_MEASURE(7850.),#9020);
#9075=MEASURE_REPRESENTATION_ITEM('density measure',
POSITIVE_RATIO_MEASURE(7850.),#9021);
#9076=PROPERTY_DEFINITION_REPRESENTATION(#9346,#9184);
#9077=PROPERTY_DEFINITION_REPRESENTATION(#9347,#9185);
#9078=PROPERTY_DEFINITION_REPRESENTATION(#9348,#9186);
#9079=PROPERTY_DEFINITION_REPRESENTATION(#9349,#9187);
#9080=PROPERTY_DEFINITION_REPRESENTATION(#9350,#9188);
#9081=PROPERTY_DEFINITION_REPRESENTATION(#9351,#9189);
#9082=PROPERTY_DEFINITION_REPRESENTATION(#9352,#9190);
#9083=PROPERTY_DEFINITION_REPRESENTATION(#9353,#9191);
#9084=PROPERTY_DEFINITION_REPRESENTATION(#9354,#9192);
#9085=PROPERTY_DEFINITION_REPRESENTATION(#9355,#9193);
#9086=PROPERTY_DEFINITION_REPRESENTATION(#9356,#9194);
#9087=PROPERTY_DEFINITION_REPRESENTATION(#9357,#9195);
#9088=PROPERTY_DEFINITION_REPRESENTATION(#9358,#9196);
#9089=PROPERTY_DEFINITION_REPRESENTATION(#9359,#9197);
#9090=PROPERTY_DEFINITION_REPRESENTATION(#9360,#9198);
#9091=PROPERTY_DEFINITION_REPRESENTATION(#9361,#9199);
#9092=PROPERTY_DEFINITION_REPRESENTATION(#9362,#9200);
#9093=PROPERTY_DEFINITION_REPRESENTATION(#9363,#9201);
#9094=PROPERTY_DEFINITION_REPRESENTATION(#9364,#9202);
#9095=PROPERTY_DEFINITION_REPRESENTATION(#9365,#9203);
#9096=PROPERTY_DEFINITION_REPRESENTATION(#9366,#9204);
#9097=PROPERTY_DEFINITION_REPRESENTATION(#9367,#9205);
#9098=PROPERTY_DEFINITION_REPRESENTATION(#9368,#9206);
#9099=PROPERTY_DEFINITION_REPRESENTATION(#9369,#9207);
#9100=PROPERTY_DEFINITION_REPRESENTATION(#9370,#9208);
#9101=PROPERTY_DEFINITION_REPRESENTATION(#9371,#9209);
#9102=PROPERTY_DEFINITION_REPRESENTATION(#9372,#9210);
#9103=PROPERTY_DEFINITION_REPRESENTATION(#9373,#9211);
#9104=PROPERTY_DEFINITION_REPRESENTATION(#9374,#9212);
#9105=PROPERTY_DEFINITION_REPRESENTATION(#9375,#9213);
#9106=PROPERTY_DEFINITION_REPRESENTATION(#9376,#9214);
#9107=PROPERTY_DEFINITION_REPRESENTATION(#9377,#9215);
#9108=PROPERTY_DEFINITION_REPRESENTATION(#9378,#9216);
#9109=PROPERTY_DEFINITION_REPRESENTATION(#9379,#9217);
#9110=PROPERTY_DEFINITION_REPRESENTATION(#9380,#9218);
#9111=PROPERTY_DEFINITION_REPRESENTATION(#9381,#9219);
#9112=PROPERTY_DEFINITION_REPRESENTATION(#9382,#9220);
#9113=PROPERTY_DEFINITION_REPRESENTATION(#9383,#9221);
#9114=PROPERTY_DEFINITION_REPRESENTATION(#9384,#9222);
#9115=PROPERTY_DEFINITION_REPRESENTATION(#9385,#9223);
#9116=PROPERTY_DEFINITION_REPRESENTATION(#9386,#9224);
#9117=PROPERTY_DEFINITION_REPRESENTATION(#9387,#9225);
#9118=PROPERTY_DEFINITION_REPRESENTATION(#9388,#9226);
#9119=PROPERTY_DEFINITION_REPRESENTATION(#9389,#9227);
#9120=PROPERTY_DEFINITION_REPRESENTATION(#9390,#9228);
#9121=PROPERTY_DEFINITION_REPRESENTATION(#9391,#9229);
#9122=PROPERTY_DEFINITION_REPRESENTATION(#9392,#9230);
#9123=PROPERTY_DEFINITION_REPRESENTATION(#9393,#9231);
#9124=PROPERTY_DEFINITION_REPRESENTATION(#9394,#9232);
#9125=PROPERTY_DEFINITION_REPRESENTATION(#9395,#9233);
#9126=PROPERTY_DEFINITION_REPRESENTATION(#9396,#9234);
#9127=PROPERTY_DEFINITION_REPRESENTATION(#9397,#9235);
#9128=PROPERTY_DEFINITION_REPRESENTATION(#9398,#9236);
#9129=PROPERTY_DEFINITION_REPRESENTATION(#9399,#9237);
#9130=PROPERTY_DEFINITION_REPRESENTATION(#9400,#9238);
#9131=PROPERTY_DEFINITION_REPRESENTATION(#9401,#9239);
#9132=PROPERTY_DEFINITION_REPRESENTATION(#9402,#9240);
#9133=PROPERTY_DEFINITION_REPRESENTATION(#9403,#9241);
#9134=PROPERTY_DEFINITION_REPRESENTATION(#9404,#9242);
#9135=PROPERTY_DEFINITION_REPRESENTATION(#9405,#9243);
#9136=PROPERTY_DEFINITION_REPRESENTATION(#9406,#9244);
#9137=PROPERTY_DEFINITION_REPRESENTATION(#9407,#9245);
#9138=PROPERTY_DEFINITION_REPRESENTATION(#9408,#9246);
#9139=PROPERTY_DEFINITION_REPRESENTATION(#9409,#9247);
#9140=PROPERTY_DEFINITION_REPRESENTATION(#9410,#9248);
#9141=PROPERTY_DEFINITION_REPRESENTATION(#9411,#9249);
#9142=PROPERTY_DEFINITION_REPRESENTATION(#9412,#9250);
#9143=PROPERTY_DEFINITION_REPRESENTATION(#9413,#9251);
#9144=PROPERTY_DEFINITION_REPRESENTATION(#9414,#9252);
#9145=PROPERTY_DEFINITION_REPRESENTATION(#9415,#9253);
#9146=PROPERTY_DEFINITION_REPRESENTATION(#9416,#9254);
#9147=PROPERTY_DEFINITION_REPRESENTATION(#9417,#9255);
#9148=PROPERTY_DEFINITION_REPRESENTATION(#9418,#9256);
#9149=PROPERTY_DEFINITION_REPRESENTATION(#9419,#9257);
#9150=PROPERTY_DEFINITION_REPRESENTATION(#9420,#9258);
#9151=PROPERTY_DEFINITION_REPRESENTATION(#9421,#9259);
#9152=PROPERTY_DEFINITION_REPRESENTATION(#9422,#9260);
#9153=PROPERTY_DEFINITION_REPRESENTATION(#9423,#9261);
#9154=PROPERTY_DEFINITION_REPRESENTATION(#9424,#9262);
#9155=PROPERTY_DEFINITION_REPRESENTATION(#9425,#9263);
#9156=PROPERTY_DEFINITION_REPRESENTATION(#9426,#9264);
#9157=PROPERTY_DEFINITION_REPRESENTATION(#9427,#9265);
#9158=PROPERTY_DEFINITION_REPRESENTATION(#9428,#9266);
#9159=PROPERTY_DEFINITION_REPRESENTATION(#9429,#9267);
#9160=PROPERTY_DEFINITION_REPRESENTATION(#9430,#9268);
#9161=PROPERTY_DEFINITION_REPRESENTATION(#9431,#9269);
#9162=PROPERTY_DEFINITION_REPRESENTATION(#9432,#9270);
#9163=PROPERTY_DEFINITION_REPRESENTATION(#9433,#9271);
#9164=PROPERTY_DEFINITION_REPRESENTATION(#9434,#9272);
#9165=PROPERTY_DEFINITION_REPRESENTATION(#9435,#9273);
#9166=PROPERTY_DEFINITION_REPRESENTATION(#9436,#9274);
#9167=PROPERTY_DEFINITION_REPRESENTATION(#9437,#9275);
#9168=PROPERTY_DEFINITION_REPRESENTATION(#9438,#9276);
#9169=PROPERTY_DEFINITION_REPRESENTATION(#9439,#9277);
#9170=PROPERTY_DEFINITION_REPRESENTATION(#9440,#9278);
#9171=PROPERTY_DEFINITION_REPRESENTATION(#9441,#9279);
#9172=PROPERTY_DEFINITION_REPRESENTATION(#9442,#9280);
#9173=PROPERTY_DEFINITION_REPRESENTATION(#9443,#9281);
#9174=PROPERTY_DEFINITION_REPRESENTATION(#9444,#9282);
#9175=PROPERTY_DEFINITION_REPRESENTATION(#9445,#9283);
#9176=PROPERTY_DEFINITION_REPRESENTATION(#9446,#9284);
#9177=PROPERTY_DEFINITION_REPRESENTATION(#9447,#9285);
#9178=PROPERTY_DEFINITION_REPRESENTATION(#9448,#9286);
#9179=PROPERTY_DEFINITION_REPRESENTATION(#9449,#9287);
#9180=PROPERTY_DEFINITION_REPRESENTATION(#9450,#9288);
#9181=PROPERTY_DEFINITION_REPRESENTATION(#9451,#9289);
#9182=PROPERTY_DEFINITION_REPRESENTATION(#9452,#9290);
#9183=PROPERTY_DEFINITION_REPRESENTATION(#9453,#9291);
#9184=REPRESENTATION('material name',(#9292),#16617);
#9185=REPRESENTATION('density',(#9022),#16617);
#9186=REPRESENTATION('material name',(#9293),#16618);
#9187=REPRESENTATION('density',(#9023),#16618);
#9188=REPRESENTATION('material name',(#9294),#16619);
#9189=REPRESENTATION('density',(#9024),#16619);
#9190=REPRESENTATION('material name',(#9295),#16620);
#9191=REPRESENTATION('density',(#9025),#16620);
#9192=REPRESENTATION('material name',(#9296),#16621);
#9193=REPRESENTATION('density',(#9026),#16621);
#9194=REPRESENTATION('material name',(#9297),#16622);
#9195=REPRESENTATION('density',(#9027),#16622);
#9196=REPRESENTATION('material name',(#9298),#16623);
#9197=REPRESENTATION('density',(#9028),#16623);
#9198=REPRESENTATION('material name',(#9299),#16624);
#9199=REPRESENTATION('density',(#9029),#16624);
#9200=REPRESENTATION('material name',(#9300),#16625);
#9201=REPRESENTATION('density',(#9030),#16625);
#9202=REPRESENTATION('material name',(#9301),#16626);
#9203=REPRESENTATION('density',(#9031),#16626);
#9204=REPRESENTATION('material name',(#9302),#16628);
#9205=REPRESENTATION('density',(#9032),#16628);
#9206=REPRESENTATION('material name',(#9303),#16629);
#9207=REPRESENTATION('density',(#9033),#16629);
#9208=REPRESENTATION('material name',(#9304),#16630);
#9209=REPRESENTATION('density',(#9034),#16630);
#9210=REPRESENTATION('material name',(#9305),#16631);
#9211=REPRESENTATION('density',(#9035),#16631);
#9212=REPRESENTATION('material name',(#9306),#16632);
#9213=REPRESENTATION('density',(#9036),#16632);
#9214=REPRESENTATION('material name',(#9307),#16633);
#9215=REPRESENTATION('density',(#9037),#16633);
#9216=REPRESENTATION('material name',(#9308),#16634);
#9217=REPRESENTATION('density',(#9038),#16634);
#9218=REPRESENTATION('material name',(#9309),#16636);
#9219=REPRESENTATION('density',(#9039),#16636);
#9220=REPRESENTATION('material name',(#9310),#16637);
#9221=REPRESENTATION('density',(#9040),#16637);
#9222=REPRESENTATION('material name',(#9311),#16638);
#9223=REPRESENTATION('density',(#9041),#16638);
#9224=REPRESENTATION('material name',(#9312),#16639);
#9225=REPRESENTATION('density',(#9042),#16639);
#9226=REPRESENTATION('material name',(#9313),#16640);
#9227=REPRESENTATION('density',(#9043),#16640);
#9228=REPRESENTATION('material name',(#9314),#16641);
#9229=REPRESENTATION('density',(#9044),#16641);
#9230=REPRESENTATION('material name',(#9315),#16642);
#9231=REPRESENTATION('density',(#9045),#16642);
#9232=REPRESENTATION('material name',(#9316),#16643);
#9233=REPRESENTATION('density',(#9046),#16643);
#9234=REPRESENTATION('material name',(#9317),#16644);
#9235=REPRESENTATION('density',(#9047),#16644);
#9236=REPRESENTATION('material name',(#9318),#16645);
#9237=REPRESENTATION('density',(#9048),#16645);
#9238=REPRESENTATION('material name',(#9319),#16646);
#9239=REPRESENTATION('density',(#9049),#16646);
#9240=REPRESENTATION('material name',(#9320),#16647);
#9241=REPRESENTATION('density',(#9050),#16647);
#9242=REPRESENTATION('material name',(#9321),#16648);
#9243=REPRESENTATION('density',(#9051),#16648);
#9244=REPRESENTATION('material name',(#9322),#16649);
#9245=REPRESENTATION('density',(#9052),#16649);
#9246=REPRESENTATION('material name',(#9323),#16651);
#9247=REPRESENTATION('density',(#9053),#16651);
#9248=REPRESENTATION('material name',(#9324),#16652);
#9249=REPRESENTATION('density',(#9054),#16652);
#9250=REPRESENTATION('material name',(#9325),#16653);
#9251=REPRESENTATION('density',(#9055),#16653);
#9252=REPRESENTATION('material name',(#9326),#16655);
#9253=REPRESENTATION('density',(#9056),#16655);
#9254=REPRESENTATION('material name',(#9327),#16656);
#9255=REPRESENTATION('density',(#9057),#16656);
#9256=REPRESENTATION('material name',(#9328),#16657);
#9257=REPRESENTATION('density',(#9058),#16657);
#9258=REPRESENTATION('material name',(#9329),#16659);
#9259=REPRESENTATION('density',(#9059),#16659);
#9260=REPRESENTATION('material name',(#9330),#16660);
#9261=REPRESENTATION('density',(#9060),#16660);
#9262=REPRESENTATION('material name',(#9331),#16661);
#9263=REPRESENTATION('density',(#9061),#16661);
#9264=REPRESENTATION('material name',(#9332),#16662);
#9265=REPRESENTATION('density',(#9062),#16662);
#9266=REPRESENTATION('material name',(#9333),#16663);
#9267=REPRESENTATION('density',(#9063),#16663);
#9268=REPRESENTATION('material name',(#9334),#16664);
#9269=REPRESENTATION('density',(#9064),#16664);
#9270=REPRESENTATION('material name',(#9335),#16665);
#9271=REPRESENTATION('density',(#9065),#16665);
#9272=REPRESENTATION('material name',(#9336),#16667);
#9273=REPRESENTATION('density',(#9066),#16667);
#9274=REPRESENTATION('material name',(#9337),#16668);
#9275=REPRESENTATION('density',(#9067),#16668);
#9276=REPRESENTATION('material name',(#9338),#16669);
#9277=REPRESENTATION('density',(#9068),#16669);
#9278=REPRESENTATION('material name',(#9339),#16670);
#9279=REPRESENTATION('density',(#9069),#16670);
#9280=REPRESENTATION('material name',(#9340),#16671);
#9281=REPRESENTATION('density',(#9070),#16671);
#9282=REPRESENTATION('material name',(#9341),#16672);
#9283=REPRESENTATION('density',(#9071),#16672);
#9284=REPRESENTATION('material name',(#9342),#16673);
#9285=REPRESENTATION('density',(#9072),#16673);
#9286=REPRESENTATION('material name',(#9343),#16675);
#9287=REPRESENTATION('density',(#9073),#16675);
#9288=REPRESENTATION('material name',(#9344),#16676);
#9289=REPRESENTATION('density',(#9074),#16676);
#9290=REPRESENTATION('material name',(#9345),#16677);
#9291=REPRESENTATION('density',(#9075),#16677);
#9292=DESCRIPTIVE_REPRESENTATION_ITEM('Steel','Steel');
#9293=DESCRIPTIVE_REPRESENTATION_ITEM('Steel','Steel');
#9294=DESCRIPTIVE_REPRESENTATION_ITEM('Steel','Steel');
#9295=DESCRIPTIVE_REPRESENTATION_ITEM('Steel','Steel');
#9296=DESCRIPTIVE_REPRESENTATION_ITEM('Steel','Steel');
#9297=DESCRIPTIVE_REPRESENTATION_ITEM('Steel','Steel');
#9298=DESCRIPTIVE_REPRESENTATION_ITEM('Steel','Steel');
#9299=DESCRIPTIVE_REPRESENTATION_ITEM('Steel','Steel');
#9300=DESCRIPTIVE_REPRESENTATION_ITEM('Steel','Steel');
#9301=DESCRIPTIVE_REPRESENTATION_ITEM('Steel','Steel');
#9302=DESCRIPTIVE_REPRESENTATION_ITEM('Steel','Steel');
#9303=DESCRIPTIVE_REPRESENTATION_ITEM('Steel','Steel');
#9304=DESCRIPTIVE_REPRESENTATION_ITEM('Steel','Steel');
#9305=DESCRIPTIVE_REPRESENTATION_ITEM('Steel','Steel');
#9306=DESCRIPTIVE_REPRESENTATION_ITEM('Steel','Steel');
#9307=DESCRIPTIVE_REPRESENTATION_ITEM('Steel','Steel');
#9308=DESCRIPTIVE_REPRESENTATION_ITEM('Steel','Steel');
#9309=DESCRIPTIVE_REPRESENTATION_ITEM('Steel','Steel');
#9310=DESCRIPTIVE_REPRESENTATION_ITEM('Steel','Steel');
#9311=DESCRIPTIVE_REPRESENTATION_ITEM('Steel','Steel');
#9312=DESCRIPTIVE_REPRESENTATION_ITEM('Steel','Steel');
#9313=DESCRIPTIVE_REPRESENTATION_ITEM('Steel','Steel');
#9314=DESCRIPTIVE_REPRESENTATION_ITEM('Steel','Steel');
#9315=DESCRIPTIVE_REPRESENTATION_ITEM('Steel','Steel');
#9316=DESCRIPTIVE_REPRESENTATION_ITEM('Steel','Steel');
#9317=DESCRIPTIVE_REPRESENTATION_ITEM('Steel','Steel');
#9318=DESCRIPTIVE_REPRESENTATION_ITEM('Steel','Steel');
#9319=DESCRIPTIVE_REPRESENTATION_ITEM('Steel','Steel');
#9320=DESCRIPTIVE_REPRESENTATION_ITEM('Steel','Steel');
#9321=DESCRIPTIVE_REPRESENTATION_ITEM('Steel','Steel');
#9322=DESCRIPTIVE_REPRESENTATION_ITEM('Steel','Steel');
#9323=DESCRIPTIVE_REPRESENTATION_ITEM('Steel','Steel');
#9324=DESCRIPTIVE_REPRESENTATION_ITEM('Steel','Steel');
#9325=DESCRIPTIVE_REPRESENTATION_ITEM('Steel','Steel');
#9326=DESCRIPTIVE_REPRESENTATION_ITEM('Steel','Steel');
#9327=DESCRIPTIVE_REPRESENTATION_ITEM('Steel','Steel');
#9328=DESCRIPTIVE_REPRESENTATION_ITEM('Steel','Steel');
#9329=DESCRIPTIVE_REPRESENTATION_ITEM('Steel','Steel');
#9330=DESCRIPTIVE_REPRESENTATION_ITEM('Steel','Steel');
#9331=DESCRIPTIVE_REPRESENTATION_ITEM('Steel','Steel');
#9332=DESCRIPTIVE_REPRESENTATION_ITEM('Steel','Steel');
#9333=DESCRIPTIVE_REPRESENTATION_ITEM('Steel','Steel');
#9334=DESCRIPTIVE_REPRESENTATION_ITEM('Steel','Steel');
#9335=DESCRIPTIVE_REPRESENTATION_ITEM('Steel','Steel');
#9336=DESCRIPTIVE_REPRESENTATION_ITEM('Steel','Steel');
#9337=DESCRIPTIVE_REPRESENTATION_ITEM('Steel','Steel');
#9338=DESCRIPTIVE_REPRESENTATION_ITEM('Steel','Steel');
#9339=DESCRIPTIVE_REPRESENTATION_ITEM('Steel','Steel');
#9340=DESCRIPTIVE_REPRESENTATION_ITEM('Steel','Steel');
#9341=DESCRIPTIVE_REPRESENTATION_ITEM('Steel','Steel');
#9342=DESCRIPTIVE_REPRESENTATION_ITEM('Steel','Steel');
#9343=DESCRIPTIVE_REPRESENTATION_ITEM('Steel','Steel');
#9344=DESCRIPTIVE_REPRESENTATION_ITEM('Steel','Steel');
#9345=DESCRIPTIVE_REPRESENTATION_ITEM('Steel','Steel');
#9346=PROPERTY_DEFINITION('material property','material name',#16976);
#9347=PROPERTY_DEFINITION('material property','density of part',#16976);
#9348=PROPERTY_DEFINITION('material property','material name',#16977);
#9349=PROPERTY_DEFINITION('material property','density of part',#16977);
#9350=PROPERTY_DEFINITION('material property','material name',#16978);
#9351=PROPERTY_DEFINITION('material property','density of part',#16978);
#9352=PROPERTY_DEFINITION('material property','material name',#16979);
#9353=PROPERTY_DEFINITION('material property','density of part',#16979);
#9354=PROPERTY_DEFINITION('material property','material name',#16980);
#9355=PROPERTY_DEFINITION('material property','density of part',#16980);
#9356=PROPERTY_DEFINITION('material property','material name',#16981);
#9357=PROPERTY_DEFINITION('material property','density of part',#16981);
#9358=PROPERTY_DEFINITION('material property','material name',#16982);
#9359=PROPERTY_DEFINITION('material property','density of part',#16982);
#9360=PROPERTY_DEFINITION('material property','material name',#16983);
#9361=PROPERTY_DEFINITION('material property','density of part',#16983);
#9362=PROPERTY_DEFINITION('material property','material name',#16984);
#9363=PROPERTY_DEFINITION('material property','density of part',#16984);
#9364=PROPERTY_DEFINITION('material property','material name',#16985);
#9365=PROPERTY_DEFINITION('material property','density of part',#16985);
#9366=PROPERTY_DEFINITION('material property','material name',#16987);
#9367=PROPERTY_DEFINITION('material property','density of part',#16987);
#9368=PROPERTY_DEFINITION('material property','material name',#16988);
#9369=PROPERTY_DEFINITION('material property','density of part',#16988);
#9370=PROPERTY_DEFINITION('material property','material name',#16989);
#9371=PROPERTY_DEFINITION('material property','density of part',#16989);
#9372=PROPERTY_DEFINITION('material property','material name',#16990);
#9373=PROPERTY_DEFINITION('material property','density of part',#16990);
#9374=PROPERTY_DEFINITION('material property','material name',#16991);
#9375=PROPERTY_DEFINITION('material property','density of part',#16991);
#9376=PROPERTY_DEFINITION('material property','material name',#16992);
#9377=PROPERTY_DEFINITION('material property','density of part',#16992);
#9378=PROPERTY_DEFINITION('material property','material name',#16993);
#9379=PROPERTY_DEFINITION('material property','density of part',#16993);
#9380=PROPERTY_DEFINITION('material property','material name',#16995);
#9381=PROPERTY_DEFINITION('material property','density of part',#16995);
#9382=PROPERTY_DEFINITION('material property','material name',#16996);
#9383=PROPERTY_DEFINITION('material property','density of part',#16996);
#9384=PROPERTY_DEFINITION('material property','material name',#16997);
#9385=PROPERTY_DEFINITION('material property','density of part',#16997);
#9386=PROPERTY_DEFINITION('material property','material name',#16998);
#9387=PROPERTY_DEFINITION('material property','density of part',#16998);
#9388=PROPERTY_DEFINITION('material property','material name',#16999);
#9389=PROPERTY_DEFINITION('material property','density of part',#16999);
#9390=PROPERTY_DEFINITION('material property','material name',#17000);
#9391=PROPERTY_DEFINITION('material property','density of part',#17000);
#9392=PROPERTY_DEFINITION('material property','material name',#17001);
#9393=PROPERTY_DEFINITION('material property','density of part',#17001);
#9394=PROPERTY_DEFINITION('material property','material name',#17002);
#9395=PROPERTY_DEFINITION('material property','density of part',#17002);
#9396=PROPERTY_DEFINITION('material property','material name',#17003);
#9397=PROPERTY_DEFINITION('material property','density of part',#17003);
#9398=PROPERTY_DEFINITION('material property','material name',#17004);
#9399=PROPERTY_DEFINITION('material property','density of part',#17004);
#9400=PROPERTY_DEFINITION('material property','material name',#17005);
#9401=PROPERTY_DEFINITION('material property','density of part',#17005);
#9402=PROPERTY_DEFINITION('material property','material name',#17006);
#9403=PROPERTY_DEFINITION('material property','density of part',#17006);
#9404=PROPERTY_DEFINITION('material property','material name',#17007);
#9405=PROPERTY_DEFINITION('material property','density of part',#17007);
#9406=PROPERTY_DEFINITION('material property','material name',#17008);
#9407=PROPERTY_DEFINITION('material property','density of part',#17008);
#9408=PROPERTY_DEFINITION('material property','material name',#17010);
#9409=PROPERTY_DEFINITION('material property','density of part',#17010);
#9410=PROPERTY_DEFINITION('material property','material name',#17011);
#9411=PROPERTY_DEFINITION('material property','density of part',#17011);
#9412=PROPERTY_DEFINITION('material property','material name',#17012);
#9413=PROPERTY_DEFINITION('material property','density of part',#17012);
#9414=PROPERTY_DEFINITION('material property','material name',#17014);
#9415=PROPERTY_DEFINITION('material property','density of part',#17014);
#9416=PROPERTY_DEFINITION('material property','material name',#17015);
#9417=PROPERTY_DEFINITION('material property','density of part',#17015);
#9418=PROPERTY_DEFINITION('material property','material name',#17016);
#9419=PROPERTY_DEFINITION('material property','density of part',#17016);
#9420=PROPERTY_DEFINITION('material property','material name',#17018);
#9421=PROPERTY_DEFINITION('material property','density of part',#17018);
#9422=PROPERTY_DEFINITION('material property','material name',#17019);
#9423=PROPERTY_DEFINITION('material property','density of part',#17019);
#9424=PROPERTY_DEFINITION('material property','material name',#17020);
#9425=PROPERTY_DEFINITION('material property','density of part',#17020);
#9426=PROPERTY_DEFINITION('material property','material name',#17021);
#9427=PROPERTY_DEFINITION('material property','density of part',#17021);
#9428=PROPERTY_DEFINITION('material property','material name',#17022);
#9429=PROPERTY_DEFINITION('material property','density of part',#17022);
#9430=PROPERTY_DEFINITION('material property','material name',#17023);
#9431=PROPERTY_DEFINITION('material property','density of part',#17023);
#9432=PROPERTY_DEFINITION('material property','material name',#17024);
#9433=PROPERTY_DEFINITION('material property','density of part',#17024);
#9434=PROPERTY_DEFINITION('material property','material name',#17026);
#9435=PROPERTY_DEFINITION('material property','density of part',#17026);
#9436=PROPERTY_DEFINITION('material property','material name',#17027);
#9437=PROPERTY_DEFINITION('material property','density of part',#17027);
#9438=PROPERTY_DEFINITION('material property','material name',#17028);
#9439=PROPERTY_DEFINITION('material property','density of part',#17028);
#9440=PROPERTY_DEFINITION('material property','material name',#17029);
#9441=PROPERTY_DEFINITION('material property','density of part',#17029);
#9442=PROPERTY_DEFINITION('material property','material name',#17030);
#9443=PROPERTY_DEFINITION('material property','density of part',#17030);
#9444=PROPERTY_DEFINITION('material property','material name',#17031);
#9445=PROPERTY_DEFINITION('material property','density of part',#17031);
#9446=PROPERTY_DEFINITION('material property','material name',#17032);
#9447=PROPERTY_DEFINITION('material property','density of part',#17032);
#9448=PROPERTY_DEFINITION('material property','material name',#17034);
#9449=PROPERTY_DEFINITION('material property','density of part',#17034);
#9450=PROPERTY_DEFINITION('material property','material name',#17035);
#9451=PROPERTY_DEFINITION('material property','density of part',#17035);
#9452=PROPERTY_DEFINITION('material property','material name',#17036);
#9453=PROPERTY_DEFINITION('material property','density of part',#17036);
#9454=AXIS2_PLACEMENT_3D('',#13531,#10630,#10631);
#9455=AXIS2_PLACEMENT_3D('',#13532,#10632,#10633);
#9456=AXIS2_PLACEMENT_3D('',#13533,#10634,#10635);
#9457=AXIS2_PLACEMENT_3D('',#13534,#10636,#10637);
#9458=AXIS2_PLACEMENT_3D('',#13536,#10638,#10639);
#9459=AXIS2_PLACEMENT_3D('',#13539,#10641,#10642);
#9460=AXIS2_PLACEMENT_3D('',#13540,#10643,#10644);
#9461=AXIS2_PLACEMENT_3D('',#13542,#10645,#10646);
#9462=AXIS2_PLACEMENT_3D('',#13545,#10648,#10649);
#9463=AXIS2_PLACEMENT_3D('',#13546,#10650,#10651);
#9464=AXIS2_PLACEMENT_3D('',#13548,#10652,#10653);
#9465=AXIS2_PLACEMENT_3D('',#13551,#10655,#10656);
#9466=AXIS2_PLACEMENT_3D('',#13552,#10657,#10658);
#9467=AXIS2_PLACEMENT_3D('',#13554,#10659,#10660);
#9468=AXIS2_PLACEMENT_3D('',#13557,#10662,#10663);
#9469=AXIS2_PLACEMENT_3D('',#13558,#10664,#10665);
#9470=AXIS2_PLACEMENT_3D('',#13560,#10666,#10667);
#9471=AXIS2_PLACEMENT_3D('',#13563,#10669,#10670);
#9472=AXIS2_PLACEMENT_3D('',#13564,#10671,#10672);
#9473=AXIS2_PLACEMENT_3D('',#13566,#10673,#10674);
#9474=AXIS2_PLACEMENT_3D('',#13569,#10676,#10677);
#9475=AXIS2_PLACEMENT_3D('',#13570,#10678,#10679);
#9476=AXIS2_PLACEMENT_3D('',#13572,#10680,#10681);
#9477=AXIS2_PLACEMENT_3D('',#13575,#10683,#10684);
#9478=AXIS2_PLACEMENT_3D('',#13576,#10685,#10686);
#9479=AXIS2_PLACEMENT_3D('',#13578,#10687,#10688);
#9480=AXIS2_PLACEMENT_3D('',#13581,#10690,#10691);
#9481=AXIS2_PLACEMENT_3D('',#13582,#10692,#10693);
#9482=AXIS2_PLACEMENT_3D('',#13584,#10694,#10695);
#9483=AXIS2_PLACEMENT_3D('',#13587,#10697,#10698);
#9484=AXIS2_PLACEMENT_3D('',#13588,#10699,#10700);
#9485=AXIS2_PLACEMENT_3D('',#13590,#10701,#10702);
#9486=AXIS2_PLACEMENT_3D('',#13593,#10704,#10705);
#9487=AXIS2_PLACEMENT_3D('',#13594,#10706,#10707);
#9488=AXIS2_PLACEMENT_3D('',#13596,#10708,#10709);
#9489=AXIS2_PLACEMENT_3D('',#13599,#10711,#10712);
#9490=AXIS2_PLACEMENT_3D('',#13600,#10713,#10714);
#9491=AXIS2_PLACEMENT_3D('',#13602,#10715,#10716);
#9492=AXIS2_PLACEMENT_3D('',#13605,#10718,#10719);
#9493=AXIS2_PLACEMENT_3D('',#13606,#10720,#10721);
#9494=AXIS2_PLACEMENT_3D('',#13615,#10726,#10727);
#9495=AXIS2_PLACEMENT_3D('',#13621,#10731,#10732);
#9496=AXIS2_PLACEMENT_3D('',#13627,#10736,#10737);
#9497=AXIS2_PLACEMENT_3D('',#13630,#10740,#10741);
#9498=AXIS2_PLACEMENT_3D('',#13631,#10742,#10743);
#9499=AXIS2_PLACEMENT_3D('',#13632,#10744,#10745);
#9500=AXIS2_PLACEMENT_3D('',#13633,#10746,#10747);
#9501=AXIS2_PLACEMENT_3D('',#13642,#10752,#10753);
#9502=AXIS2_PLACEMENT_3D('',#13648,#10757,#10758);
#9503=AXIS2_PLACEMENT_3D('',#13654,#10762,#10763);
#9504=AXIS2_PLACEMENT_3D('',#13657,#10766,#10767);
#9505=AXIS2_PLACEMENT_3D('',#13658,#10768,#10769);
#9506=AXIS2_PLACEMENT_3D('',#13659,#10770,#10771);
#9507=AXIS2_PLACEMENT_3D('',#13660,#10772,#10773);
#9508=AXIS2_PLACEMENT_3D('',#13669,#10778,#10779);
#9509=AXIS2_PLACEMENT_3D('',#13675,#10783,#10784);
#9510=AXIS2_PLACEMENT_3D('',#13681,#10788,#10789);
#9511=AXIS2_PLACEMENT_3D('',#13684,#10792,#10793);
#9512=AXIS2_PLACEMENT_3D('',#13685,#10794,#10795);
#9513=AXIS2_PLACEMENT_3D('',#13686,#10796,#10797);
#9514=AXIS2_PLACEMENT_3D('',#13687,#10798,#10799);
#9515=AXIS2_PLACEMENT_3D('',#13765,#10801,#10802);
#9516=AXIS2_PLACEMENT_3D('',#13767,#10803,#10804);
#9517=AXIS2_PLACEMENT_3D('',#13770,#10806,#10807);
#9518=AXIS2_PLACEMENT_3D('',#13771,#10808,#10809);
#9519=AXIS2_PLACEMENT_3D('',#13772,#10810,#10811);
#9520=AXIS2_PLACEMENT_3D('',#13774,#10812,#10813);
#9521=AXIS2_PLACEMENT_3D('',#13777,#10815,#10816);
#9522=AXIS2_PLACEMENT_3D('',#13778,#10817,#10818);
#9523=AXIS2_PLACEMENT_3D('',#13779,#10819,#10820);
#9524=AXIS2_PLACEMENT_3D('',#13781,#10821,#10822);
#9525=AXIS2_PLACEMENT_3D('',#13784,#10824,#10825);
#9526=AXIS2_PLACEMENT_3D('',#13785,#10826,#10827);
#9527=AXIS2_PLACEMENT_3D('',#13786,#10828,#10829);
#9528=AXIS2_PLACEMENT_3D('',#13788,#10830,#10831);
#9529=AXIS2_PLACEMENT_3D('',#13791,#10833,#10834);
#9530=AXIS2_PLACEMENT_3D('',#13792,#10835,#10836);
#9531=AXIS2_PLACEMENT_3D('',#13793,#10837,#10838);
#9532=AXIS2_PLACEMENT_3D('',#13796,#10839,#10840);
#9533=AXIS2_PLACEMENT_3D('',#13797,#10841,#10842);
#9534=AXIS2_PLACEMENT_3D('',#13798,#10843,#10844);
#9535=AXIS2_PLACEMENT_3D('',#13802,#10846,#10847);
#9536=AXIS2_PLACEMENT_3D('',#13804,#10849,#10850);
#9537=AXIS2_PLACEMENT_3D('',#13809,#10852,#10853);
#9538=AXIS2_PLACEMENT_3D('',#13812,#10855,#10856);
#9539=AXIS2_PLACEMENT_3D('',#13813,#10857,#10858);
#9540=AXIS2_PLACEMENT_3D('',#13814,#10859,#10860);
#9541=AXIS2_PLACEMENT_3D('',#13815,#10861,#10862);
#9542=AXIS2_PLACEMENT_3D('',#13820,#10864,#10865);
#9543=AXIS2_PLACEMENT_3D('',#13823,#10867,#10868);
#9544=AXIS2_PLACEMENT_3D('',#13824,#10869,#10870);
#9545=AXIS2_PLACEMENT_3D('',#13825,#10871,#10872);
#9546=AXIS2_PLACEMENT_3D('',#13826,#10873,#10874);
#9547=AXIS2_PLACEMENT_3D('',#13831,#10876,#10877);
#9548=AXIS2_PLACEMENT_3D('',#13834,#10879,#10880);
#9549=AXIS2_PLACEMENT_3D('',#13835,#10881,#10882);
#9550=AXIS2_PLACEMENT_3D('',#13836,#10883,#10884);
#9551=AXIS2_PLACEMENT_3D('',#13837,#10885,#10886);
#9552=AXIS2_PLACEMENT_3D('',#13839,#10887,#10888);
#9553=AXIS2_PLACEMENT_3D('',#13842,#10890,#10891);
#9554=AXIS2_PLACEMENT_3D('',#13843,#10892,#10893);
#9555=AXIS2_PLACEMENT_3D('',#13844,#10894,#10895);
#9556=AXIS2_PLACEMENT_3D('',#13845,#10896,#10897);
#9557=AXIS2_PLACEMENT_3D('',#13846,#10898,#10899);
#9558=AXIS2_PLACEMENT_3D('',#13847,#10900,#10901);
#9559=AXIS2_PLACEMENT_3D('',#13849,#10902,#10903);
#9560=AXIS2_PLACEMENT_3D('',#13851,#10904,#10905);
#9561=AXIS2_PLACEMENT_3D('',#13853,#10906,#10907);
#9562=AXIS2_PLACEMENT_3D('',#13855,#10908,#10909);
#9563=AXIS2_PLACEMENT_3D('',#13857,#10910,#10911);
#9564=AXIS2_PLACEMENT_3D('',#13858,#10912,#10913);
#9565=AXIS2_PLACEMENT_3D('',#13860,#10914,#10915);
#9566=AXIS2_PLACEMENT_3D('',#13862,#10917,#10918);
#9567=AXIS2_PLACEMENT_3D('',#13864,#10919,#10920);
#9568=AXIS2_PLACEMENT_3D('',#13866,#10922,#10923);
#9569=AXIS2_PLACEMENT_3D('',#13868,#10924,#10925);
#9570=AXIS2_PLACEMENT_3D('',#13870,#10927,#10928);
#9571=AXIS2_PLACEMENT_3D('',#13872,#10929,#10930);
#9572=AXIS2_PLACEMENT_3D('',#13874,#10932,#10933);
#9573=AXIS2_PLACEMENT_3D('',#13876,#10934,#10935);
#9574=AXIS2_PLACEMENT_3D('',#13879,#10937,#10938);
#9575=AXIS2_PLACEMENT_3D('',#13880,#10939,#10940);
#9576=AXIS2_PLACEMENT_3D('',#13882,#10941,#10942);
#9577=AXIS2_PLACEMENT_3D('',#13883,#10943,#10944);
#9578=AXIS2_PLACEMENT_3D('',#13886,#10946,#10947);
#9579=AXIS2_PLACEMENT_3D('',#13887,#10948,#10949);
#9580=AXIS2_PLACEMENT_3D('',#13890,#10951,#10952);
#9581=AXIS2_PLACEMENT_3D('',#13891,#10953,#10954);
#9582=AXIS2_PLACEMENT_3D('',#13892,#10955,#10956);
#9583=AXIS2_PLACEMENT_3D('',#13893,#10957,#10958);
#9584=AXIS2_PLACEMENT_3D('',#13894,#10959,#10960);
#9585=AXIS2_PLACEMENT_3D('',#13896,#10961,#10962);
#9586=AXIS2_PLACEMENT_3D('',#13899,#10964,#10965);
#9587=AXIS2_PLACEMENT_3D('',#13900,#10966,#10967);
#9588=AXIS2_PLACEMENT_3D('',#13902,#10968,#10969);
#9589=AXIS2_PLACEMENT_3D('',#13903,#10970,#10971);
#9590=AXIS2_PLACEMENT_3D('',#13905,#10972,#10973);
#9591=AXIS2_PLACEMENT_3D('',#13908,#10975,#10976);
#9592=AXIS2_PLACEMENT_3D('',#13909,#10977,#10978);
#9593=AXIS2_PLACEMENT_3D('',#13911,#10979,#10980);
#9594=AXIS2_PLACEMENT_3D('',#13912,#10981,#10982);
#9595=AXIS2_PLACEMENT_3D('',#13914,#10983,#10984);
#9596=AXIS2_PLACEMENT_3D('',#13917,#10986,#10987);
#9597=AXIS2_PLACEMENT_3D('',#13918,#10988,#10989);
#9598=AXIS2_PLACEMENT_3D('',#13920,#10990,#10991);
#9599=AXIS2_PLACEMENT_3D('',#13921,#10992,#10993);
#9600=AXIS2_PLACEMENT_3D('',#13923,#10994,#10995);
#9601=AXIS2_PLACEMENT_3D('',#13926,#10997,#10998);
#9602=AXIS2_PLACEMENT_3D('',#13927,#10999,#11000);
#9603=AXIS2_PLACEMENT_3D('',#13929,#11001,#11002);
#9604=AXIS2_PLACEMENT_3D('',#13930,#11003,#11004);
#9605=AXIS2_PLACEMENT_3D('',#13932,#11005,#11006);
#9606=AXIS2_PLACEMENT_3D('',#13934,#11008,#11009);
#9607=AXIS2_PLACEMENT_3D('',#13936,#11010,#11011);
#9608=AXIS2_PLACEMENT_3D('',#13938,#11013,#11014);
#9609=AXIS2_PLACEMENT_3D('',#13940,#11015,#11016);
#9610=AXIS2_PLACEMENT_3D('',#13942,#11018,#11019);
#9611=AXIS2_PLACEMENT_3D('',#13944,#11020,#11021);
#9612=AXIS2_PLACEMENT_3D('',#13946,#11023,#11024);
#9613=AXIS2_PLACEMENT_3D('',#13948,#11025,#11026);
#9614=AXIS2_PLACEMENT_3D('',#13951,#11028,#11029);
#9615=AXIS2_PLACEMENT_3D('',#13952,#11030,#11031);
#9616=AXIS2_PLACEMENT_3D('',#13954,#11032,#11033);
#9617=AXIS2_PLACEMENT_3D('',#13955,#11034,#11035);
#9618=AXIS2_PLACEMENT_3D('',#13957,#11036,#11037);
#9619=AXIS2_PLACEMENT_3D('',#13959,#11039,#11040);
#9620=AXIS2_PLACEMENT_3D('',#13961,#11041,#11042);
#9621=AXIS2_PLACEMENT_3D('',#13964,#11044,#11045);
#9622=AXIS2_PLACEMENT_3D('',#13965,#11046,#11047);
#9623=AXIS2_PLACEMENT_3D('',#13966,#11048,#11049);
#9624=AXIS2_PLACEMENT_3D('',#13967,#11050,#11051);
#9625=AXIS2_PLACEMENT_3D('',#13968,#11052,#11053);
#9626=AXIS2_PLACEMENT_3D('',#13973,#11055,#11056);
#9627=AXIS2_PLACEMENT_3D('',#13976,#11058,#11059);
#9628=AXIS2_PLACEMENT_3D('',#13977,#11060,#11061);
#9629=AXIS2_PLACEMENT_3D('',#13982,#11063,#11064);
#9630=AXIS2_PLACEMENT_3D('',#13985,#11066,#11067);
#9631=AXIS2_PLACEMENT_3D('',#13986,#11068,#11069);
#9632=AXIS2_PLACEMENT_3D('',#13990,#11071,#11072);
#9633=AXIS2_PLACEMENT_3D('',#13991,#11073,#11074);
#9634=AXIS2_PLACEMENT_3D('',#14001,#11075,#11076);
#9635=AXIS2_PLACEMENT_3D('',#14023,#11078,#11079);
#9636=AXIS2_PLACEMENT_3D('',#14024,#11080,#11081);
#9637=AXIS2_PLACEMENT_3D('',#14026,#11083,#11084);
#9638=AXIS2_PLACEMENT_3D('',#14027,#11085,#11086);
#9639=AXIS2_PLACEMENT_3D('',#14029,#11088,#11089);
#9640=AXIS2_PLACEMENT_3D('',#14030,#11090,#11091);
#9641=AXIS2_PLACEMENT_3D('',#14032,#11092,#11093);
#9642=AXIS2_PLACEMENT_3D('',#14033,#11094,#11095);
#9643=AXIS2_PLACEMENT_3D('',#14034,#11096,#11097);
#9644=AXIS2_PLACEMENT_3D('',#14036,#11099,#11100);
#9645=AXIS2_PLACEMENT_3D('',#14037,#11101,#11102);
#9646=AXIS2_PLACEMENT_3D('',#14039,#11103,#11104);
#9647=AXIS2_PLACEMENT_3D('',#14040,#11105,#11106);
#9648=AXIS2_PLACEMENT_3D('',#14051,#11113,#11114);
#9649=AXIS2_PLACEMENT_3D('',#14053,#11115,#11116);
#9650=AXIS2_PLACEMENT_3D('',#14055,#11118,#11119);
#9651=AXIS2_PLACEMENT_3D('',#14057,#11120,#11121);
#9652=AXIS2_PLACEMENT_3D('',#14059,#11123,#11124);
#9653=AXIS2_PLACEMENT_3D('',#14061,#11125,#11126);
#9654=AXIS2_PLACEMENT_3D('',#14065,#11129,#11130);
#9655=AXIS2_PLACEMENT_3D('',#14066,#11131,#11132);
#9656=AXIS2_PLACEMENT_3D('',#14072,#11136,#11137);
#9657=AXIS2_PLACEMENT_3D('',#14076,#11140,#11141);
#9658=AXIS2_PLACEMENT_3D('',#14080,#11144,#11145);
#9659=AXIS2_PLACEMENT_3D('',#14082,#11147,#11148);
#9660=AXIS2_PLACEMENT_3D('',#14083,#11149,#11150);
#9661=AXIS2_PLACEMENT_3D('',#14084,#11151,#11152);
#9662=AXIS2_PLACEMENT_3D('',#14089,#11154,#11155);
#9663=AXIS2_PLACEMENT_3D('',#14092,#11157,#11158);
#9664=AXIS2_PLACEMENT_3D('',#14093,#11159,#11160);
#9665=AXIS2_PLACEMENT_3D('',#14098,#11162,#11163);
#9666=AXIS2_PLACEMENT_3D('',#14101,#11165,#11166);
#9667=AXIS2_PLACEMENT_3D('',#14102,#11167,#11168);
#9668=AXIS2_PLACEMENT_3D('',#14106,#11170,#11171);
#9669=AXIS2_PLACEMENT_3D('',#14107,#11172,#11173);
#9670=AXIS2_PLACEMENT_3D('',#14117,#11174,#11175);
#9671=AXIS2_PLACEMENT_3D('',#14139,#11177,#11178);
#9672=AXIS2_PLACEMENT_3D('',#14140,#11179,#11180);
#9673=AXIS2_PLACEMENT_3D('',#14142,#11182,#11183);
#9674=AXIS2_PLACEMENT_3D('',#14143,#11184,#11185);
#9675=AXIS2_PLACEMENT_3D('',#14145,#11187,#11188);
#9676=AXIS2_PLACEMENT_3D('',#14146,#11189,#11190);
#9677=AXIS2_PLACEMENT_3D('',#14148,#11191,#11192);
#9678=AXIS2_PLACEMENT_3D('',#14149,#11193,#11194);
#9679=AXIS2_PLACEMENT_3D('',#14150,#11195,#11196);
#9680=AXIS2_PLACEMENT_3D('',#14152,#11198,#11199);
#9681=AXIS2_PLACEMENT_3D('',#14153,#11200,#11201);
#9682=AXIS2_PLACEMENT_3D('',#14155,#11202,#11203);
#9683=AXIS2_PLACEMENT_3D('',#14156,#11204,#11205);
#9684=AXIS2_PLACEMENT_3D('',#14167,#11212,#11213);
#9685=AXIS2_PLACEMENT_3D('',#14169,#11214,#11215);
#9686=AXIS2_PLACEMENT_3D('',#14171,#11217,#11218);
#9687=AXIS2_PLACEMENT_3D('',#14173,#11219,#11220);
#9688=AXIS2_PLACEMENT_3D('',#14175,#11222,#11223);
#9689=AXIS2_PLACEMENT_3D('',#14177,#11224,#11225);
#9690=AXIS2_PLACEMENT_3D('',#14181,#11228,#11229);
#9691=AXIS2_PLACEMENT_3D('',#14182,#11230,#11231);
#9692=AXIS2_PLACEMENT_3D('',#14188,#11235,#11236);
#9693=AXIS2_PLACEMENT_3D('',#14192,#11239,#11240);
#9694=AXIS2_PLACEMENT_3D('',#14196,#11243,#11244);
#9695=AXIS2_PLACEMENT_3D('',#14198,#11246,#11247);
#9696=AXIS2_PLACEMENT_3D('',#14199,#11248,#11249);
#9697=AXIS2_PLACEMENT_3D('',#14200,#11250,#11251);
#9698=AXIS2_PLACEMENT_3D('',#14205,#11253,#11254);
#9699=AXIS2_PLACEMENT_3D('',#14208,#11256,#11257);
#9700=AXIS2_PLACEMENT_3D('',#14209,#11258,#11259);
#9701=AXIS2_PLACEMENT_3D('',#14213,#11261,#11262);
#9702=AXIS2_PLACEMENT_3D('',#14214,#11263,#11264);
#9703=AXIS2_PLACEMENT_3D('',#14227,#11265,#11266);
#9704=AXIS2_PLACEMENT_3D('',#14230,#11268,#11269);
#9705=AXIS2_PLACEMENT_3D('',#14232,#11270,#11271);
#9706=AXIS2_PLACEMENT_3D('',#14243,#11272,#11273);
#9707=AXIS2_PLACEMENT_3D('',#14245,#11275,#11276);
#9708=AXIS2_PLACEMENT_3D('',#14247,#11277,#11278);
#9709=AXIS2_PLACEMENT_3D('',#14250,#11280,#11281);
#9710=AXIS2_PLACEMENT_3D('',#14252,#11283,#11284);
#9711=AXIS2_PLACEMENT_3D('',#14254,#11285,#11286);
#9712=AXIS2_PLACEMENT_3D('',#14255,#11287,#11288);
#9713=AXIS2_PLACEMENT_3D('',#14256,#11289,#11290);
#9714=AXIS2_PLACEMENT_3D('',#14258,#11292,#11293);
#9715=AXIS2_PLACEMENT_3D('',#14259,#11294,#11295);
#9716=AXIS2_PLACEMENT_3D('',#14261,#11296,#11297);
#9717=AXIS2_PLACEMENT_3D('',#14262,#11298,#11299);
#9718=AXIS2_PLACEMENT_3D('',#14273,#11306,#11307);
#9719=AXIS2_PLACEMENT_3D('',#14275,#11308,#11309);
#9720=AXIS2_PLACEMENT_3D('',#14277,#11311,#11312);
#9721=AXIS2_PLACEMENT_3D('',#14279,#11313,#11314);
#9722=AXIS2_PLACEMENT_3D('',#14281,#11316,#11317);
#9723=AXIS2_PLACEMENT_3D('',#14283,#11318,#11319);
#9724=AXIS2_PLACEMENT_3D('',#14286,#11321,#11322);
#9725=AXIS2_PLACEMENT_3D('',#14287,#11323,#11324);
#9726=AXIS2_PLACEMENT_3D('',#14293,#11328,#11329);
#9727=AXIS2_PLACEMENT_3D('',#14297,#11332,#11333);
#9728=AXIS2_PLACEMENT_3D('',#14301,#11336,#11337);
#9729=AXIS2_PLACEMENT_3D('',#14303,#11339,#11340);
#9730=AXIS2_PLACEMENT_3D('',#14304,#11341,#11342);
#9731=AXIS2_PLACEMENT_3D('',#14305,#11343,#11344);
#9732=AXIS2_PLACEMENT_3D('',#14310,#11346,#11347);
#9733=AXIS2_PLACEMENT_3D('',#14313,#11349,#11350);
#9734=AXIS2_PLACEMENT_3D('',#14314,#11351,#11352);
#9735=AXIS2_PLACEMENT_3D('',#14318,#11354,#11355);
#9736=AXIS2_PLACEMENT_3D('',#14319,#11356,#11357);
#9737=AXIS2_PLACEMENT_3D('',#14332,#11358,#11359);
#9738=AXIS2_PLACEMENT_3D('',#14335,#11361,#11362);
#9739=AXIS2_PLACEMENT_3D('',#14337,#11363,#11364);
#9740=AXIS2_PLACEMENT_3D('',#14348,#11365,#11366);
#9741=AXIS2_PLACEMENT_3D('',#14350,#11368,#11369);
#9742=AXIS2_PLACEMENT_3D('',#14352,#11370,#11371);
#9743=AXIS2_PLACEMENT_3D('',#14355,#11373,#11374);
#9744=AXIS2_PLACEMENT_3D('',#14357,#11376,#11377);
#9745=AXIS2_PLACEMENT_3D('',#14359,#11378,#11379);
#9746=AXIS2_PLACEMENT_3D('',#14360,#11380,#11381);
#9747=AXIS2_PLACEMENT_3D('',#14361,#11382,#11383);
#9748=AXIS2_PLACEMENT_3D('',#14363,#11385,#11386);
#9749=AXIS2_PLACEMENT_3D('',#14364,#11387,#11388);
#9750=AXIS2_PLACEMENT_3D('',#14366,#11389,#11390);
#9751=AXIS2_PLACEMENT_3D('',#14367,#11391,#11392);
#9752=AXIS2_PLACEMENT_3D('',#14378,#11399,#11400);
#9753=AXIS2_PLACEMENT_3D('',#14380,#11401,#11402);
#9754=AXIS2_PLACEMENT_3D('',#14382,#11404,#11405);
#9755=AXIS2_PLACEMENT_3D('',#14384,#11406,#11407);
#9756=AXIS2_PLACEMENT_3D('',#14386,#11409,#11410);
#9757=AXIS2_PLACEMENT_3D('',#14388,#11411,#11412);
#9758=AXIS2_PLACEMENT_3D('',#14391,#11414,#11415);
#9759=AXIS2_PLACEMENT_3D('',#14392,#11416,#11417);
#9760=AXIS2_PLACEMENT_3D('',#14398,#11421,#11422);
#9761=AXIS2_PLACEMENT_3D('',#14402,#11425,#11426);
#9762=AXIS2_PLACEMENT_3D('',#14406,#11429,#11430);
#9763=AXIS2_PLACEMENT_3D('',#14408,#11432,#11433);
#9764=AXIS2_PLACEMENT_3D('',#14409,#11434,#11435);
#9765=AXIS2_PLACEMENT_3D('',#14410,#11436,#11437);
#9766=AXIS2_PLACEMENT_3D('',#14419,#11442,#11443);
#9767=AXIS2_PLACEMENT_3D('',#14425,#11447,#11448);
#9768=AXIS2_PLACEMENT_3D('',#14431,#11452,#11453);
#9769=AXIS2_PLACEMENT_3D('',#14437,#11457,#11458);
#9770=AXIS2_PLACEMENT_3D('',#14443,#11462,#11463);
#9771=AXIS2_PLACEMENT_3D('',#14446,#11466,#11467);
#9772=AXIS2_PLACEMENT_3D('',#14447,#11468,#11469);
#9773=AXIS2_PLACEMENT_3D('',#14448,#11470,#11471);
#9774=AXIS2_PLACEMENT_3D('',#14450,#11472,#11473);
#9775=AXIS2_PLACEMENT_3D('',#14451,#11474,#11475);
#9776=AXIS2_PLACEMENT_3D('',#14453,#11476,#11477);
#9777=AXIS2_PLACEMENT_3D('',#14454,#11478,#11479);
#9778=AXIS2_PLACEMENT_3D('',#14456,#11480,#11481);
#9779=AXIS2_PLACEMENT_3D('',#14458,#11483,#11484);
#9780=AXIS2_PLACEMENT_3D('',#14460,#11485,#11486);
#9781=AXIS2_PLACEMENT_3D('',#14462,#11488,#11489);
#9782=AXIS2_PLACEMENT_3D('',#14464,#11490,#11491);
#9783=AXIS2_PLACEMENT_3D('',#14466,#11493,#11494);
#9784=AXIS2_PLACEMENT_3D('',#14468,#11495,#11496);
#9785=AXIS2_PLACEMENT_3D('',#14469,#11497,#11498);
#9786=AXIS2_PLACEMENT_3D('',#14471,#11499,#11500);
#9787=AXIS2_PLACEMENT_3D('',#14473,#11502,#11503);
#9788=AXIS2_PLACEMENT_3D('',#14475,#11505,#11506);
#9789=AXIS2_PLACEMENT_3D('',#14476,#11507,#11508);
#9790=AXIS2_PLACEMENT_3D('',#14477,#11509,#11510);
#9791=AXIS2_PLACEMENT_3D('',#14480,#11511,#11512);
#9792=AXIS2_PLACEMENT_3D('',#14481,#11513,#11514);
#9793=AXIS2_PLACEMENT_3D('',#14483,#11515,#11516);
#9794=AXIS2_PLACEMENT_3D('',#14485,#11517,#11518);
#9795=AXIS2_PLACEMENT_3D('',#14486,#11519,#11520);
#9796=AXIS2_PLACEMENT_3D('',#14487,#11521,#11522);
#9797=AXIS2_PLACEMENT_3D('',#14490,#11524,#11525);
#9798=AXIS2_PLACEMENT_3D('',#14491,#11526,#11527);
#9799=AXIS2_PLACEMENT_3D('',#14493,#11528,#11529);
#9800=AXIS2_PLACEMENT_3D('',#14496,#11531,#11532);
#9801=AXIS2_PLACEMENT_3D('',#14497,#11533,#11534);
#9802=AXIS2_PLACEMENT_3D('',#14500,#11536,#11537);
#9803=AXIS2_PLACEMENT_3D('',#14501,#11538,#11539);
#9804=AXIS2_PLACEMENT_3D('',#14502,#11540,#11541);
#9805=AXIS2_PLACEMENT_3D('',#14504,#11542,#11543);
#9806=AXIS2_PLACEMENT_3D('',#14506,#11545,#11546);
#9807=AXIS2_PLACEMENT_3D('',#14508,#11547,#11548);
#9808=AXIS2_PLACEMENT_3D('',#14509,#11549,#11550);
#9809=AXIS2_PLACEMENT_3D('',#14511,#11552,#11553);
#9810=AXIS2_PLACEMENT_3D('',#14512,#11554,#11555);
#9811=AXIS2_PLACEMENT_3D('',#14515,#11556,#11557);
#9812=AXIS2_PLACEMENT_3D('',#14516,#11558,#11559);
#9813=AXIS2_PLACEMENT_3D('',#14518,#11560,#11561);
#9814=AXIS2_PLACEMENT_3D('',#14520,#11562,#11563);
#9815=AXIS2_PLACEMENT_3D('',#14521,#11564,#11565);
#9816=AXIS2_PLACEMENT_3D('',#14522,#11566,#11567);
#9817=AXIS2_PLACEMENT_3D('',#14524,#11568,#11569);
#9818=AXIS2_PLACEMENT_3D('',#14526,#11571,#11572);
#9819=AXIS2_PLACEMENT_3D('',#14528,#11573,#11574);
#9820=AXIS2_PLACEMENT_3D('',#14530,#11575,#11576);
#9821=AXIS2_PLACEMENT_3D('',#14531,#11577,#11578);
#9822=AXIS2_PLACEMENT_3D('',#14533,#11579,#11580);
#9823=AXIS2_PLACEMENT_3D('',#14535,#11582,#11583);
#9824=AXIS2_PLACEMENT_3D('',#14537,#11584,#11585);
#9825=AXIS2_PLACEMENT_3D('',#14539,#11587,#11588);
#9826=AXIS2_PLACEMENT_3D('',#14541,#11589,#11590);
#9827=AXIS2_PLACEMENT_3D('',#14543,#11592,#11593);
#9828=AXIS2_PLACEMENT_3D('',#14544,#11594,#11595);
#9829=AXIS2_PLACEMENT_3D('',#14546,#11597,#11598);
#9830=AXIS2_PLACEMENT_3D('',#14547,#11599,#11600);
#9831=AXIS2_PLACEMENT_3D('',#14550,#11601,#11602);
#9832=AXIS2_PLACEMENT_3D('',#14551,#11603,#11604);
#9833=AXIS2_PLACEMENT_3D('',#14554,#11605,#11606);
#9834=AXIS2_PLACEMENT_3D('',#14555,#11607,#11608);
#9835=AXIS2_PLACEMENT_3D('',#14558,#11609,#11610);
#9836=AXIS2_PLACEMENT_3D('',#14559,#11611,#11612);
#9837=AXIS2_PLACEMENT_3D('',#14562,#11613,#11614);
#9838=AXIS2_PLACEMENT_3D('',#14563,#11615,#11616);
#9839=AXIS2_PLACEMENT_3D('',#14566,#11617,#11618);
#9840=AXIS2_PLACEMENT_3D('',#14567,#11619,#11620);
#9841=AXIS2_PLACEMENT_3D('',#14570,#11621,#11622);
#9842=AXIS2_PLACEMENT_3D('',#14571,#11623,#11624);
#9843=AXIS2_PLACEMENT_3D('',#14574,#11625,#11626);
#9844=AXIS2_PLACEMENT_3D('',#14575,#11627,#11628);
#9845=AXIS2_PLACEMENT_3D('',#14578,#11629,#11630);
#9846=AXIS2_PLACEMENT_3D('',#14579,#11631,#11632);
#9847=AXIS2_PLACEMENT_3D('',#14580,#11633,#11634);
#9848=AXIS2_PLACEMENT_3D('',#14606,#11635,#11636);
#9849=AXIS2_PLACEMENT_3D('',#14630,#11637,#11638);
#9850=AXIS2_PLACEMENT_3D('',#14631,#11639,#11640);
#9851=AXIS2_PLACEMENT_3D('',#14633,#11641,#11642);
#9852=AXIS2_PLACEMENT_3D('',#14658,#11643,#11644);
#9853=AXIS2_PLACEMENT_3D('',#14683,#11645,#11646);
#9854=AXIS2_PLACEMENT_3D('',#14699,#11648,#11649);
#9855=AXIS2_PLACEMENT_3D('',#14714,#11650,#11651);
#9856=AXIS2_PLACEMENT_3D('',#14739,#11652,#11653);
#9857=AXIS2_PLACEMENT_3D('',#14764,#11654,#11655);
#9858=AXIS2_PLACEMENT_3D('',#14789,#11656,#11657);
#9859=AXIS2_PLACEMENT_3D('',#14813,#11658,#11659);
#9860=AXIS2_PLACEMENT_3D('',#14814,#11660,#11661);
#9861=AXIS2_PLACEMENT_3D('',#14816,#11662,#11663);
#9862=AXIS2_PLACEMENT_3D('',#14817,#11664,#11665);
#9863=AXIS2_PLACEMENT_3D('',#14818,#11666,#11667);
#9864=AXIS2_PLACEMENT_3D('',#14842,#11668,#11669);
#9865=AXIS2_PLACEMENT_3D('',#14843,#11670,#11671);
#9866=AXIS2_PLACEMENT_3D('',#14845,#11672,#11673);
#9867=AXIS2_PLACEMENT_3D('',#14846,#11674,#11675);
#9868=AXIS2_PLACEMENT_3D('',#14847,#11676,#11677);
#9869=AXIS2_PLACEMENT_3D('',#14871,#11678,#11679);
#9870=AXIS2_PLACEMENT_3D('',#14872,#11680,#11681);
#9871=AXIS2_PLACEMENT_3D('',#14874,#11682,#11683);
#9872=AXIS2_PLACEMENT_3D('',#14875,#11684,#11685);
#9873=AXIS2_PLACEMENT_3D('',#14876,#11686,#11687);
#9874=AXIS2_PLACEMENT_3D('',#14891,#11688,#11689);
#9875=AXIS2_PLACEMENT_3D('',#14904,#11690,#11691);
#9876=AXIS2_PLACEMENT_3D('',#14906,#11692,#11693);
#9877=AXIS2_PLACEMENT_3D('',#14907,#11694,#11695);
#9878=AXIS2_PLACEMENT_3D('',#14908,#11696,#11697);
#9879=AXIS2_PLACEMENT_3D('',#14932,#11698,#11699);
#9880=AXIS2_PLACEMENT_3D('',#14933,#11700,#11701);
#9881=AXIS2_PLACEMENT_3D('',#14935,#11702,#11703);
#9882=AXIS2_PLACEMENT_3D('',#14936,#11704,#11705);
#9883=AXIS2_PLACEMENT_3D('',#14937,#11706,#11707);
#9884=AXIS2_PLACEMENT_3D('',#14961,#11708,#11709);
#9885=AXIS2_PLACEMENT_3D('',#14962,#11710,#11711);
#9886=AXIS2_PLACEMENT_3D('',#14964,#11712,#11713);
#9887=AXIS2_PLACEMENT_3D('',#14965,#11714,#11715);
#9888=AXIS2_PLACEMENT_3D('',#14966,#11716,#11717);
#9889=AXIS2_PLACEMENT_3D('',#14990,#11718,#11719);
#9890=AXIS2_PLACEMENT_3D('',#14991,#11720,#11721);
#9891=AXIS2_PLACEMENT_3D('',#14993,#11722,#11723);
#9892=AXIS2_PLACEMENT_3D('',#14996,#11725,#11726);
#9893=AXIS2_PLACEMENT_3D('',#15020,#11727,#11728);
#9894=AXIS2_PLACEMENT_3D('',#15021,#11729,#11730);
#9895=AXIS2_PLACEMENT_3D('',#15022,#11731,#11732);
#9896=AXIS2_PLACEMENT_3D('',#15023,#11733,#11734);
#9897=AXIS2_PLACEMENT_3D('',#15024,#11735,#11736);
#9898=AXIS2_PLACEMENT_3D('',#15025,#11737,#11738);
#9899=AXIS2_PLACEMENT_3D('',#15026,#11739,#11740);
#9900=AXIS2_PLACEMENT_3D('',#15027,#11741,#11742);
#9901=AXIS2_PLACEMENT_3D('',#15028,#11743,#11744);
#9902=AXIS2_PLACEMENT_3D('',#15030,#11745,#11746);
#9903=AXIS2_PLACEMENT_3D('',#15032,#11747,#11748);
#9904=AXIS2_PLACEMENT_3D('',#15033,#11749,#11750);
#9905=AXIS2_PLACEMENT_3D('',#15035,#11751,#11752);
#9906=AXIS2_PLACEMENT_3D('',#15037,#11754,#11755);
#9907=AXIS2_PLACEMENT_3D('',#15039,#11756,#11757);
#9908=AXIS2_PLACEMENT_3D('',#15040,#11758,#11759);
#9909=AXIS2_PLACEMENT_3D('',#15042,#11761,#11762);
#9910=AXIS2_PLACEMENT_3D('',#15044,#11763,#11764);
#9911=AXIS2_PLACEMENT_3D('',#15046,#11765,#11766);
#9912=AXIS2_PLACEMENT_3D('',#15047,#11767,#11768);
#9913=AXIS2_PLACEMENT_3D('',#15049,#11769,#11770);
#9914=AXIS2_PLACEMENT_3D('',#15051,#11772,#11773);
#9915=AXIS2_PLACEMENT_3D('',#15053,#11774,#11775);
#9916=AXIS2_PLACEMENT_3D('',#15054,#11776,#11777);
#9917=AXIS2_PLACEMENT_3D('',#15056,#11779,#11780);
#9918=AXIS2_PLACEMENT_3D('',#15057,#11781,#11782);
#9919=AXIS2_PLACEMENT_3D('',#15058,#11783,#11784);
#9920=AXIS2_PLACEMENT_3D('',#15059,#11785,#11786);
#9921=AXIS2_PLACEMENT_3D('',#15060,#11787,#11788);
#9922=AXIS2_PLACEMENT_3D('',#15061,#11789,#11790);
#9923=AXIS2_PLACEMENT_3D('',#15062,#11791,#11792);
#9924=AXIS2_PLACEMENT_3D('',#15064,#11793,#11794);
#9925=AXIS2_PLACEMENT_3D('',#15065,#11795,#11796);
#9926=AXIS2_PLACEMENT_3D('',#15067,#11797,#11798);
#9927=AXIS2_PLACEMENT_3D('',#15070,#11800,#11801);
#9928=AXIS2_PLACEMENT_3D('',#15071,#11802,#11803);
#9929=AXIS2_PLACEMENT_3D('',#15073,#11805,#11806);
#9930=AXIS2_PLACEMENT_3D('',#15074,#11807,#11808);
#9931=AXIS2_PLACEMENT_3D('',#15075,#11809,#11810);
#9932=AXIS2_PLACEMENT_3D('',#15084,#11815,#11816);
#9933=AXIS2_PLACEMENT_3D('',#15090,#11820,#11821);
#9934=AXIS2_PLACEMENT_3D('',#15096,#11825,#11826);
#9935=AXIS2_PLACEMENT_3D('',#15102,#11830,#11831);
#9936=AXIS2_PLACEMENT_3D('',#15108,#11835,#11836);
#9937=AXIS2_PLACEMENT_3D('',#15111,#11839,#11840);
#9938=AXIS2_PLACEMENT_3D('',#15112,#11841,#11842);
#9939=AXIS2_PLACEMENT_3D('',#15114,#11843,#11844);
#9940=AXIS2_PLACEMENT_3D('',#15115,#11845,#11846);
#9941=AXIS2_PLACEMENT_3D('',#15117,#11847,#11848);
#9942=AXIS2_PLACEMENT_3D('',#15119,#11850,#11851);
#9943=AXIS2_PLACEMENT_3D('',#15121,#11852,#11853);
#9944=AXIS2_PLACEMENT_3D('',#15123,#11855,#11856);
#9945=AXIS2_PLACEMENT_3D('',#15125,#11857,#11858);
#9946=AXIS2_PLACEMENT_3D('',#15127,#11860,#11861);
#9947=AXIS2_PLACEMENT_3D('',#15128,#11862,#11863);
#9948=AXIS2_PLACEMENT_3D('',#15129,#11864,#11865);
#9949=AXIS2_PLACEMENT_3D('',#15130,#11866,#11867);
#9950=AXIS2_PLACEMENT_3D('',#15132,#11868,#11869);
#9951=AXIS2_PLACEMENT_3D('',#15135,#11871,#11872);
#9952=AXIS2_PLACEMENT_3D('',#15136,#11873,#11874);
#9953=AXIS2_PLACEMENT_3D('',#15138,#11875,#11876);
#9954=AXIS2_PLACEMENT_3D('',#15141,#11878,#11879);
#9955=AXIS2_PLACEMENT_3D('',#15142,#11880,#11881);
#9956=AXIS2_PLACEMENT_3D('',#15144,#11882,#11883);
#9957=AXIS2_PLACEMENT_3D('',#15147,#11885,#11886);
#9958=AXIS2_PLACEMENT_3D('',#15148,#11887,#11888);
#9959=AXIS2_PLACEMENT_3D('',#15153,#11890,#11891);
#9960=AXIS2_PLACEMENT_3D('',#15156,#11893,#11894);
#9961=AXIS2_PLACEMENT_3D('',#15157,#11895,#11896);
#9962=AXIS2_PLACEMENT_3D('',#15163,#11900,#11901);
#9963=AXIS2_PLACEMENT_3D('',#15167,#11903,#11904);
#9964=AXIS2_PLACEMENT_3D('',#15171,#11906,#11907);
#9965=AXIS2_PLACEMENT_3D('',#15175,#11909,#11910);
#9966=AXIS2_PLACEMENT_3D('',#15179,#11912,#11913);
#9967=AXIS2_PLACEMENT_3D('',#15182,#11915,#11916);
#9968=AXIS2_PLACEMENT_3D('',#15183,#11917,#11918);
#9969=AXIS2_PLACEMENT_3D('',#15187,#11921,#11922);
#9970=AXIS2_PLACEMENT_3D('',#15190,#11924,#11925);
#9971=AXIS2_PLACEMENT_3D('',#15191,#11926,#11927);
#9972=AXIS2_PLACEMENT_3D('',#15193,#11928,#11929);
#9973=AXIS2_PLACEMENT_3D('',#15195,#11931,#11932);
#9974=AXIS2_PLACEMENT_3D('',#15200,#11935,#11936);
#9975=AXIS2_PLACEMENT_3D('',#15201,#11937,#11938);
#9976=AXIS2_PLACEMENT_3D('',#15205,#11941,#11942);
#9977=AXIS2_PLACEMENT_3D('',#15209,#11944,#11945);
#9978=AXIS2_PLACEMENT_3D('',#15212,#11947,#11948);
#9979=AXIS2_PLACEMENT_3D('',#15215,#11950,#11951);
#9980=AXIS2_PLACEMENT_3D('',#15216,#11952,#11953);
#9981=AXIS2_PLACEMENT_3D('',#15217,#11954,#11955);
#9982=AXIS2_PLACEMENT_3D('',#15220,#11958,#11959);
#9983=AXIS2_PLACEMENT_3D('',#15222,#11961,#11962);
#9984=AXIS2_PLACEMENT_3D('',#15223,#11963,#11964);
#9985=AXIS2_PLACEMENT_3D('',#15224,#11965,#11966);
#9986=AXIS2_PLACEMENT_3D('',#15226,#11967,#11968);
#9987=AXIS2_PLACEMENT_3D('',#15228,#11969,#11970);
#9988=AXIS2_PLACEMENT_3D('',#15229,#11971,#11972);
#9989=AXIS2_PLACEMENT_3D('',#15231,#11974,#11975);
#9990=AXIS2_PLACEMENT_3D('',#15234,#11977,#11978);
#9991=AXIS2_PLACEMENT_3D('',#15235,#11979,#11980);
#9992=AXIS2_PLACEMENT_3D('',#15236,#11981,#11982);
#9993=AXIS2_PLACEMENT_3D('',#15237,#11983,#11984);
#9994=AXIS2_PLACEMENT_3D('',#15239,#11985,#11986);
#9995=AXIS2_PLACEMENT_3D('',#15242,#11988,#11989);
#9996=AXIS2_PLACEMENT_3D('',#15243,#11990,#11991);
#9997=AXIS2_PLACEMENT_3D('',#15244,#11992,#11993);
#9998=AXIS2_PLACEMENT_3D('',#15246,#11994,#11995);
#9999=AXIS2_PLACEMENT_3D('',#15249,#11997,#11998);
#10000=AXIS2_PLACEMENT_3D('',#15250,#11999,#12000);
#10001=AXIS2_PLACEMENT_3D('',#15251,#12001,#12002);
#10002=AXIS2_PLACEMENT_3D('',#15252,#12003,#12004);
#10003=AXIS2_PLACEMENT_3D('',#15253,#12005,#12006);
#10004=AXIS2_PLACEMENT_3D('',#15255,#12007,#12008);
#10005=AXIS2_PLACEMENT_3D('',#15258,#12010,#12011);
#10006=AXIS2_PLACEMENT_3D('',#15259,#12012,#12013);
#10007=AXIS2_PLACEMENT_3D('',#15261,#12014,#12015);
#10008=AXIS2_PLACEMENT_3D('',#15264,#12017,#12018);
#10009=AXIS2_PLACEMENT_3D('',#15265,#12019,#12020);
#10010=AXIS2_PLACEMENT_3D('',#15266,#12021,#12022);
#10011=AXIS2_PLACEMENT_3D('',#15267,#12023,#12024);
#10012=AXIS2_PLACEMENT_3D('',#15268,#12025,#12026);
#10013=AXIS2_PLACEMENT_3D('',#15272,#12028,#12029);
#10014=AXIS2_PLACEMENT_3D('',#15273,#12030,#12031);
#10015=AXIS2_PLACEMENT_3D('',#15290,#12032,#12033);
#10016=AXIS2_PLACEMENT_3D('',#15347,#12035,#12036);
#10017=AXIS2_PLACEMENT_3D('',#15349,#12038,#12039);
#10018=AXIS2_PLACEMENT_3D('',#15351,#12040,#12041);
#10019=AXIS2_PLACEMENT_3D('',#15354,#12043,#12044);
#10020=AXIS2_PLACEMENT_3D('',#15355,#12045,#12046);
#10021=AXIS2_PLACEMENT_3D('',#15357,#12047,#12048);
#10022=AXIS2_PLACEMENT_3D('',#15360,#12050,#12051);
#10023=AXIS2_PLACEMENT_3D('',#15361,#12052,#12053);
#10024=AXIS2_PLACEMENT_3D('',#15362,#12054,#12055);
#10025=AXIS2_PLACEMENT_3D('',#15363,#12056,#12057);
#10026=AXIS2_PLACEMENT_3D('',#15364,#12058,#12059);
#10027=AXIS2_PLACEMENT_3D('',#15366,#12060,#12061);
#10028=AXIS2_PLACEMENT_3D('',#15369,#12063,#12064);
#10029=AXIS2_PLACEMENT_3D('',#15370,#12065,#12066);
#10030=AXIS2_PLACEMENT_3D('',#15371,#12067,#12068);
#10031=AXIS2_PLACEMENT_3D('',#15373,#12069,#12070);
#10032=AXIS2_PLACEMENT_3D('',#15375,#12071,#12072);
#10033=AXIS2_PLACEMENT_3D('',#15376,#12073,#12074);
#10034=AXIS2_PLACEMENT_3D('',#15378,#12075,#12076);
#10035=AXIS2_PLACEMENT_3D('',#15380,#12077,#12078);
#10036=AXIS2_PLACEMENT_3D('',#15381,#12079,#12080);
#10037=AXIS2_PLACEMENT_3D('',#15383,#12082,#12083);
#10038=AXIS2_PLACEMENT_3D('',#15386,#12085,#12086);
#10039=AXIS2_PLACEMENT_3D('',#15387,#12087,#12088);
#10040=AXIS2_PLACEMENT_3D('',#15389,#12089,#12090);
#10041=AXIS2_PLACEMENT_3D('',#15391,#12092,#12093);
#10042=AXIS2_PLACEMENT_3D('',#15392,#12094,#12095);
#10043=AXIS2_PLACEMENT_3D('',#15393,#12096,#12097);
#10044=AXIS2_PLACEMENT_3D('',#15394,#12098,#12099);
#10045=AXIS2_PLACEMENT_3D('',#15396,#12100,#12101);
#10046=AXIS2_PLACEMENT_3D('',#15399,#12103,#12104);
#10047=AXIS2_PLACEMENT_3D('',#15400,#12105,#12106);
#10048=AXIS2_PLACEMENT_3D('',#15402,#12107,#12108);
#10049=AXIS2_PLACEMENT_3D('',#15405,#12110,#12111);
#10050=AXIS2_PLACEMENT_3D('',#15406,#12112,#12113);
#10051=AXIS2_PLACEMENT_3D('',#15407,#12114,#12115);
#10052=AXIS2_PLACEMENT_3D('',#15408,#12116,#12117);
#10053=AXIS2_PLACEMENT_3D('',#15409,#12118,#12119);
#10054=AXIS2_PLACEMENT_3D('',#15411,#12120,#12121);
#10055=AXIS2_PLACEMENT_3D('',#15414,#12123,#12124);
#10056=AXIS2_PLACEMENT_3D('',#15415,#12125,#12126);
#10057=AXIS2_PLACEMENT_3D('',#15417,#12127,#12128);
#10058=AXIS2_PLACEMENT_3D('',#15420,#12130,#12131);
#10059=AXIS2_PLACEMENT_3D('',#15421,#12132,#12133);
#10060=AXIS2_PLACEMENT_3D('',#15422,#12134,#12135);
#10061=AXIS2_PLACEMENT_3D('',#15423,#12136,#12137);
#10062=AXIS2_PLACEMENT_3D('',#15424,#12138,#12139);
#10063=AXIS2_PLACEMENT_3D('',#15426,#12140,#12141);
#10064=AXIS2_PLACEMENT_3D('',#15429,#12143,#12144);
#10065=AXIS2_PLACEMENT_3D('',#15430,#12145,#12146);
#10066=AXIS2_PLACEMENT_3D('',#15432,#12147,#12148);
#10067=AXIS2_PLACEMENT_3D('',#15435,#12150,#12151);
#10068=AXIS2_PLACEMENT_3D('',#15436,#12152,#12153);
#10069=AXIS2_PLACEMENT_3D('',#15437,#12154,#12155);
#10070=AXIS2_PLACEMENT_3D('',#15438,#12156,#12157);
#10071=AXIS2_PLACEMENT_3D('',#15439,#12158,#12159);
#10072=AXIS2_PLACEMENT_3D('',#15441,#12160,#12161);
#10073=AXIS2_PLACEMENT_3D('',#15444,#12163,#12164);
#10074=AXIS2_PLACEMENT_3D('',#15445,#12165,#12166);
#10075=AXIS2_PLACEMENT_3D('',#15446,#12167,#12168);
#10076=AXIS2_PLACEMENT_3D('',#15448,#12169,#12170);
#10077=AXIS2_PLACEMENT_3D('',#15450,#12171,#12172);
#10078=AXIS2_PLACEMENT_3D('',#15451,#12173,#12174);
#10079=AXIS2_PLACEMENT_3D('',#15453,#12175,#12176);
#10080=AXIS2_PLACEMENT_3D('',#15455,#12177,#12178);
#10081=AXIS2_PLACEMENT_3D('',#15456,#12179,#12180);
#10082=AXIS2_PLACEMENT_3D('',#15458,#12182,#12183);
#10083=AXIS2_PLACEMENT_3D('',#15461,#12185,#12186);
#10084=AXIS2_PLACEMENT_3D('',#15462,#12187,#12188);
#10085=AXIS2_PLACEMENT_3D('',#15464,#12189,#12190);
#10086=AXIS2_PLACEMENT_3D('',#15466,#12192,#12193);
#10087=AXIS2_PLACEMENT_3D('',#15467,#12194,#12195);
#10088=AXIS2_PLACEMENT_3D('',#15468,#12196,#12197);
#10089=AXIS2_PLACEMENT_3D('',#15469,#12198,#12199);
#10090=AXIS2_PLACEMENT_3D('',#15471,#12200,#12201);
#10091=AXIS2_PLACEMENT_3D('',#15474,#12203,#12204);
#10092=AXIS2_PLACEMENT_3D('',#15475,#12205,#12206);
#10093=AXIS2_PLACEMENT_3D('',#15477,#12207,#12208);
#10094=AXIS2_PLACEMENT_3D('',#15480,#12210,#12211);
#10095=AXIS2_PLACEMENT_3D('',#15481,#12212,#12213);
#10096=AXIS2_PLACEMENT_3D('',#15482,#12214,#12215);
#10097=AXIS2_PLACEMENT_3D('',#15483,#12216,#12217);
#10098=AXIS2_PLACEMENT_3D('',#15484,#12218,#12219);
#10099=AXIS2_PLACEMENT_3D('',#15486,#12220,#12221);
#10100=AXIS2_PLACEMENT_3D('',#15489,#12223,#12224);
#10101=AXIS2_PLACEMENT_3D('',#15490,#12225,#12226);
#10102=AXIS2_PLACEMENT_3D('',#15492,#12227,#12228);
#10103=AXIS2_PLACEMENT_3D('',#15495,#12230,#12231);
#10104=AXIS2_PLACEMENT_3D('',#15496,#12232,#12233);
#10105=AXIS2_PLACEMENT_3D('',#15497,#12234,#12235);
#10106=AXIS2_PLACEMENT_3D('',#15498,#12236,#12237);
#10107=AXIS2_PLACEMENT_3D('',#15499,#12238,#12239);
#10108=AXIS2_PLACEMENT_3D('',#15501,#12240,#12241);
#10109=AXIS2_PLACEMENT_3D('',#15504,#12243,#12244);
#10110=AXIS2_PLACEMENT_3D('',#15505,#12245,#12246);
#10111=AXIS2_PLACEMENT_3D('',#15507,#12247,#12248);
#10112=AXIS2_PLACEMENT_3D('',#15510,#12250,#12251);
#10113=AXIS2_PLACEMENT_3D('',#15511,#12252,#12253);
#10114=AXIS2_PLACEMENT_3D('',#15512,#12254,#12255);
#10115=AXIS2_PLACEMENT_3D('',#15513,#12256,#12257);
#10116=AXIS2_PLACEMENT_3D('',#15514,#12258,#12259);
#10117=AXIS2_PLACEMENT_3D('',#15516,#12260,#12261);
#10118=AXIS2_PLACEMENT_3D('',#15517,#12262,#12263);
#10119=AXIS2_PLACEMENT_3D('',#15519,#12264,#12265);
#10120=AXIS2_PLACEMENT_3D('',#15521,#12267,#12268);
#10121=AXIS2_PLACEMENT_3D('',#15523,#12269,#12270);
#10122=AXIS2_PLACEMENT_3D('',#15525,#12272,#12273);
#10123=AXIS2_PLACEMENT_3D('',#15527,#12274,#12275);
#10124=AXIS2_PLACEMENT_3D('',#15529,#12277,#12278);
#10125=AXIS2_PLACEMENT_3D('',#15531,#12279,#12280);
#10126=AXIS2_PLACEMENT_3D('',#15532,#12281,#12282);
#10127=AXIS2_PLACEMENT_3D('',#15534,#12283,#12284);
#10128=AXIS2_PLACEMENT_3D('',#15536,#12286,#12287);
#10129=AXIS2_PLACEMENT_3D('',#15538,#12288,#12289);
#10130=AXIS2_PLACEMENT_3D('',#15540,#12291,#12292);
#10131=AXIS2_PLACEMENT_3D('',#15542,#12293,#12294);
#10132=AXIS2_PLACEMENT_3D('',#15544,#12296,#12297);
#10133=AXIS2_PLACEMENT_3D('',#15545,#12298,#12299);
#10134=AXIS2_PLACEMENT_3D('',#15554,#12304,#12305);
#10135=AXIS2_PLACEMENT_3D('',#15560,#12309,#12310);
#10136=AXIS2_PLACEMENT_3D('',#15566,#12314,#12315);
#10137=AXIS2_PLACEMENT_3D('',#15572,#12319,#12320);
#10138=AXIS2_PLACEMENT_3D('',#15578,#12324,#12325);
#10139=AXIS2_PLACEMENT_3D('',#15581,#12328,#12329);
#10140=AXIS2_PLACEMENT_3D('',#15582,#12330,#12331);
#10141=AXIS2_PLACEMENT_3D('',#15583,#12332,#12333);
#10142=AXIS2_PLACEMENT_3D('',#15584,#12334,#12335);
#10143=AXIS2_PLACEMENT_3D('',#15586,#12336,#12337);
#10144=AXIS2_PLACEMENT_3D('',#15587,#12338,#12339);
#10145=AXIS2_PLACEMENT_3D('',#15596,#12344,#12345);
#10146=AXIS2_PLACEMENT_3D('',#15602,#12349,#12350);
#10147=AXIS2_PLACEMENT_3D('',#15608,#12354,#12355);
#10148=AXIS2_PLACEMENT_3D('',#15614,#12359,#12360);
#10149=AXIS2_PLACEMENT_3D('',#15620,#12364,#12365);
#10150=AXIS2_PLACEMENT_3D('',#15623,#12368,#12369);
#10151=AXIS2_PLACEMENT_3D('',#15624,#12370,#12371);
#10152=AXIS2_PLACEMENT_3D('',#15626,#12372,#12373);
#10153=AXIS2_PLACEMENT_3D('',#15627,#12374,#12375);
#10154=AXIS2_PLACEMENT_3D('',#15629,#12376,#12377);
#10155=AXIS2_PLACEMENT_3D('',#15631,#12379,#12380);
#10156=AXIS2_PLACEMENT_3D('',#15633,#12382,#12383);
#10157=AXIS2_PLACEMENT_3D('',#15634,#12384,#12385);
#10158=AXIS2_PLACEMENT_3D('',#15635,#12386,#12387);
#10159=AXIS2_PLACEMENT_3D('',#15637,#12388,#12389);
#10160=AXIS2_PLACEMENT_3D('',#15640,#12391,#12392);
#10161=AXIS2_PLACEMENT_3D('',#15641,#12393,#12394);
#10162=AXIS2_PLACEMENT_3D('',#15643,#12395,#12396);
#10163=AXIS2_PLACEMENT_3D('',#15646,#12398,#12399);
#10164=AXIS2_PLACEMENT_3D('',#15647,#12400,#12401);
#10165=AXIS2_PLACEMENT_3D('',#15652,#12403,#12404);
#10166=AXIS2_PLACEMENT_3D('',#15655,#12406,#12407);
#10167=AXIS2_PLACEMENT_3D('',#15656,#12408,#12409);
#10168=AXIS2_PLACEMENT_3D('',#15662,#12413,#12414);
#10169=AXIS2_PLACEMENT_3D('',#15665,#12416,#12417);
#10170=AXIS2_PLACEMENT_3D('',#15666,#12418,#12419);
#10171=AXIS2_PLACEMENT_3D('',#15670,#12422,#12423);
#10172=AXIS2_PLACEMENT_3D('',#15671,#12424,#12425);
#10173=AXIS2_PLACEMENT_3D('',#15672,#12426,#12427);
#10174=AXIS2_PLACEMENT_3D('',#15673,#12428,#12429);
#10175=AXIS2_PLACEMENT_3D('',#15674,#12430,#12431);
#10176=AXIS2_PLACEMENT_3D('',#15676,#12432,#12433);
#10177=AXIS2_PLACEMENT_3D('',#15679,#12435,#12436);
#10178=AXIS2_PLACEMENT_3D('',#15680,#12437,#12438);
#10179=AXIS2_PLACEMENT_3D('',#15682,#12439,#12440);
#10180=AXIS2_PLACEMENT_3D('',#15685,#12442,#12443);
#10181=AXIS2_PLACEMENT_3D('',#15686,#12444,#12445);
#10182=AXIS2_PLACEMENT_3D('',#15687,#12446,#12447);
#10183=AXIS2_PLACEMENT_3D('',#15688,#12448,#12449);
#10184=AXIS2_PLACEMENT_3D('',#15689,#12450,#12451);
#10185=AXIS2_PLACEMENT_3D('',#15691,#12452,#12453);
#10186=AXIS2_PLACEMENT_3D('',#15694,#12455,#12456);
#10187=AXIS2_PLACEMENT_3D('',#15695,#12457,#12458);
#10188=AXIS2_PLACEMENT_3D('',#15697,#12459,#12460);
#10189=AXIS2_PLACEMENT_3D('',#15700,#12462,#12463);
#10190=AXIS2_PLACEMENT_3D('',#15701,#12464,#12465);
#10191=AXIS2_PLACEMENT_3D('',#15702,#12466,#12467);
#10192=AXIS2_PLACEMENT_3D('',#15703,#12468,#12469);
#10193=AXIS2_PLACEMENT_3D('',#15704,#12470,#12471);
#10194=AXIS2_PLACEMENT_3D('',#15705,#12472,#12473);
#10195=AXIS2_PLACEMENT_3D('',#15706,#12474,#12475);
#10196=AXIS2_PLACEMENT_3D('',#15707,#12476,#12477);
#10197=AXIS2_PLACEMENT_3D('',#15708,#12478,#12479);
#10198=AXIS2_PLACEMENT_3D('',#15710,#12480,#12481);
#10199=AXIS2_PLACEMENT_3D('',#15713,#12483,#12484);
#10200=AXIS2_PLACEMENT_3D('',#15714,#12485,#12486);
#10201=AXIS2_PLACEMENT_3D('',#15716,#12487,#12488);
#10202=AXIS2_PLACEMENT_3D('',#15719,#12490,#12491);
#10203=AXIS2_PLACEMENT_3D('',#15720,#12492,#12493);
#10204=AXIS2_PLACEMENT_3D('',#15725,#12495,#12496);
#10205=AXIS2_PLACEMENT_3D('',#15728,#12498,#12499);
#10206=AXIS2_PLACEMENT_3D('',#15729,#12500,#12501);
#10207=AXIS2_PLACEMENT_3D('',#15735,#12505,#12506);
#10208=AXIS2_PLACEMENT_3D('',#15738,#12508,#12509);
#10209=AXIS2_PLACEMENT_3D('',#15739,#12510,#12511);
#10210=AXIS2_PLACEMENT_3D('',#15743,#12514,#12515);
#10211=AXIS2_PLACEMENT_3D('',#15744,#12516,#12517);
#10212=AXIS2_PLACEMENT_3D('',#15745,#12518,#12519);
#10213=AXIS2_PLACEMENT_3D('',#15746,#12520,#12521);
#10214=AXIS2_PLACEMENT_3D('',#15747,#12522,#12523);
#10215=AXIS2_PLACEMENT_3D('',#15749,#12524,#12525);
#10216=AXIS2_PLACEMENT_3D('',#15752,#12527,#12528);
#10217=AXIS2_PLACEMENT_3D('',#15753,#12529,#12530);
#10218=AXIS2_PLACEMENT_3D('',#15755,#12531,#12532);
#10219=AXIS2_PLACEMENT_3D('',#15758,#12534,#12535);
#10220=AXIS2_PLACEMENT_3D('',#15759,#12536,#12537);
#10221=AXIS2_PLACEMENT_3D('',#15760,#12538,#12539);
#10222=AXIS2_PLACEMENT_3D('',#15761,#12540,#12541);
#10223=AXIS2_PLACEMENT_3D('',#15762,#12542,#12543);
#10224=AXIS2_PLACEMENT_3D('',#15764,#12544,#12545);
#10225=AXIS2_PLACEMENT_3D('',#15767,#12547,#12548);
#10226=AXIS2_PLACEMENT_3D('',#15768,#12549,#12550);
#10227=AXIS2_PLACEMENT_3D('',#15770,#12551,#12552);
#10228=AXIS2_PLACEMENT_3D('',#15773,#12554,#12555);
#10229=AXIS2_PLACEMENT_3D('',#15774,#12556,#12557);
#10230=AXIS2_PLACEMENT_3D('',#15775,#12558,#12559);
#10231=AXIS2_PLACEMENT_3D('',#15776,#12560,#12561);
#10232=AXIS2_PLACEMENT_3D('',#15777,#12562,#12563);
#10233=AXIS2_PLACEMENT_3D('',#15778,#12564,#12565);
#10234=AXIS2_PLACEMENT_3D('',#15779,#12566,#12567);
#10235=AXIS2_PLACEMENT_3D('',#15780,#12568,#12569);
#10236=AXIS2_PLACEMENT_3D('',#15781,#12570,#12571);
#10237=AXIS2_PLACEMENT_3D('',#15783,#12572,#12573);
#10238=AXIS2_PLACEMENT_3D('',#15786,#12575,#12576);
#10239=AXIS2_PLACEMENT_3D('',#15787,#12577,#12578);
#10240=AXIS2_PLACEMENT_3D('',#15788,#12579,#12580);
#10241=AXIS2_PLACEMENT_3D('',#15790,#12581,#12582);
#10242=AXIS2_PLACEMENT_3D('',#15793,#12584,#12585);
#10243=AXIS2_PLACEMENT_3D('',#15794,#12586,#12587);
#10244=AXIS2_PLACEMENT_3D('',#15796,#12588,#12589);
#10245=AXIS2_PLACEMENT_3D('',#15799,#12591,#12592);
#10246=AXIS2_PLACEMENT_3D('',#15800,#12593,#12594);
#10247=AXIS2_PLACEMENT_3D('',#15802,#12595,#12596);
#10248=AXIS2_PLACEMENT_3D('',#15805,#12598,#12599);
#10249=AXIS2_PLACEMENT_3D('',#15806,#12600,#12601);
#10250=AXIS2_PLACEMENT_3D('',#15808,#12602,#12603);
#10251=AXIS2_PLACEMENT_3D('',#15811,#12605,#12606);
#10252=AXIS2_PLACEMENT_3D('',#15812,#12607,#12608);
#10253=AXIS2_PLACEMENT_3D('',#15814,#12609,#12610);
#10254=AXIS2_PLACEMENT_3D('',#15817,#12612,#12613);
#10255=AXIS2_PLACEMENT_3D('',#15818,#12614,#12615);
#10256=AXIS2_PLACEMENT_3D('',#15827,#12620,#12621);
#10257=AXIS2_PLACEMENT_3D('',#15833,#12625,#12626);
#10258=AXIS2_PLACEMENT_3D('',#15839,#12630,#12631);
#10259=AXIS2_PLACEMENT_3D('',#15842,#12634,#12635);
#10260=AXIS2_PLACEMENT_3D('',#15843,#12636,#12637);
#10261=AXIS2_PLACEMENT_3D('',#15844,#12638,#12639);
#10262=AXIS2_PLACEMENT_3D('',#15845,#12640,#12641);
#10263=AXIS2_PLACEMENT_3D('',#15847,#12642,#12643);
#10264=AXIS2_PLACEMENT_3D('',#15850,#12645,#12646);
#10265=AXIS2_PLACEMENT_3D('',#15851,#12647,#12648);
#10266=AXIS2_PLACEMENT_3D('',#15853,#12649,#12650);
#10267=AXIS2_PLACEMENT_3D('',#15856,#12652,#12653);
#10268=AXIS2_PLACEMENT_3D('',#15857,#12654,#12655);
#10269=AXIS2_PLACEMENT_3D('',#15859,#12656,#12657);
#10270=AXIS2_PLACEMENT_3D('',#15862,#12659,#12660);
#10271=AXIS2_PLACEMENT_3D('',#15863,#12661,#12662);
#10272=AXIS2_PLACEMENT_3D('',#15865,#12663,#12664);
#10273=AXIS2_PLACEMENT_3D('',#15868,#12666,#12667);
#10274=AXIS2_PLACEMENT_3D('',#15869,#12668,#12669);
#10275=AXIS2_PLACEMENT_3D('',#15871,#12670,#12671);
#10276=AXIS2_PLACEMENT_3D('',#15874,#12673,#12674);
#10277=AXIS2_PLACEMENT_3D('',#15875,#12675,#12676);
#10278=AXIS2_PLACEMENT_3D('',#15884,#12681,#12682);
#10279=AXIS2_PLACEMENT_3D('',#15890,#12686,#12687);
#10280=AXIS2_PLACEMENT_3D('',#15896,#12691,#12692);
#10281=AXIS2_PLACEMENT_3D('',#15899,#12695,#12696);
#10282=AXIS2_PLACEMENT_3D('',#15900,#12697,#12698);
#10283=AXIS2_PLACEMENT_3D('',#15901,#12699,#12700);
#10284=AXIS2_PLACEMENT_3D('',#15902,#12701,#12702);
#10285=AXIS2_PLACEMENT_3D('',#15904,#12703,#12704);
#10286=AXIS2_PLACEMENT_3D('',#15907,#12706,#12707);
#10287=AXIS2_PLACEMENT_3D('',#15908,#12708,#12709);
#10288=AXIS2_PLACEMENT_3D('',#15910,#12710,#12711);
#10289=AXIS2_PLACEMENT_3D('',#15913,#12713,#12714);
#10290=AXIS2_PLACEMENT_3D('',#15914,#12715,#12716);
#10291=AXIS2_PLACEMENT_3D('',#15916,#12717,#12718);
#10292=AXIS2_PLACEMENT_3D('',#15919,#12720,#12721);
#10293=AXIS2_PLACEMENT_3D('',#15920,#12722,#12723);
#10294=AXIS2_PLACEMENT_3D('',#15922,#12724,#12725);
#10295=AXIS2_PLACEMENT_3D('',#15925,#12727,#12728);
#10296=AXIS2_PLACEMENT_3D('',#15926,#12729,#12730);
#10297=AXIS2_PLACEMENT_3D('',#15928,#12731,#12732);
#10298=AXIS2_PLACEMENT_3D('',#15931,#12734,#12735);
#10299=AXIS2_PLACEMENT_3D('',#15932,#12736,#12737);
#10300=AXIS2_PLACEMENT_3D('',#15941,#12742,#12743);
#10301=AXIS2_PLACEMENT_3D('',#15947,#12747,#12748);
#10302=AXIS2_PLACEMENT_3D('',#15953,#12752,#12753);
#10303=AXIS2_PLACEMENT_3D('',#15956,#12756,#12757);
#10304=AXIS2_PLACEMENT_3D('',#15957,#12758,#12759);
#10305=AXIS2_PLACEMENT_3D('',#15958,#12760,#12761);
#10306=AXIS2_PLACEMENT_3D('',#15959,#12762,#12763);
#10307=AXIS2_PLACEMENT_3D('',#15961,#12764,#12765);
#10308=AXIS2_PLACEMENT_3D('',#15964,#12767,#12768);
#10309=AXIS2_PLACEMENT_3D('',#15965,#12769,#12770);
#10310=AXIS2_PLACEMENT_3D('',#15966,#12771,#12772);
#10311=AXIS2_PLACEMENT_3D('',#15968,#12773,#12774);
#10312=AXIS2_PLACEMENT_3D('',#15970,#12775,#12776);
#10313=AXIS2_PLACEMENT_3D('',#15971,#12777,#12778);
#10314=AXIS2_PLACEMENT_3D('',#15973,#12779,#12780);
#10315=AXIS2_PLACEMENT_3D('',#15975,#12781,#12782);
#10316=AXIS2_PLACEMENT_3D('',#15976,#12783,#12784);
#10317=AXIS2_PLACEMENT_3D('',#15978,#12786,#12787);
#10318=AXIS2_PLACEMENT_3D('',#15981,#12789,#12790);
#10319=AXIS2_PLACEMENT_3D('',#15982,#12791,#12792);
#10320=AXIS2_PLACEMENT_3D('',#15984,#12793,#12794);
#10321=AXIS2_PLACEMENT_3D('',#15986,#12796,#12797);
#10322=AXIS2_PLACEMENT_3D('',#15987,#12798,#12799);
#10323=AXIS2_PLACEMENT_3D('',#15988,#12800,#12801);
#10324=AXIS2_PLACEMENT_3D('',#15989,#12802,#12803);
#10325=AXIS2_PLACEMENT_3D('',#15991,#12804,#12805);
#10326=AXIS2_PLACEMENT_3D('',#15994,#12807,#12808);
#10327=AXIS2_PLACEMENT_3D('',#15995,#12809,#12810);
#10328=AXIS2_PLACEMENT_3D('',#15997,#12811,#12812);
#10329=AXIS2_PLACEMENT_3D('',#16000,#12814,#12815);
#10330=AXIS2_PLACEMENT_3D('',#16001,#12816,#12817);
#10331=AXIS2_PLACEMENT_3D('',#16002,#12818,#12819);
#10332=AXIS2_PLACEMENT_3D('',#16003,#12820,#12821);
#10333=AXIS2_PLACEMENT_3D('',#16004,#12822,#12823);
#10334=AXIS2_PLACEMENT_3D('',#16006,#12824,#12825);
#10335=AXIS2_PLACEMENT_3D('',#16009,#12827,#12828);
#10336=AXIS2_PLACEMENT_3D('',#16010,#12829,#12830);
#10337=AXIS2_PLACEMENT_3D('',#16012,#12831,#12832);
#10338=AXIS2_PLACEMENT_3D('',#16015,#12834,#12835);
#10339=AXIS2_PLACEMENT_3D('',#16016,#12836,#12837);
#10340=AXIS2_PLACEMENT_3D('',#16017,#12838,#12839);
#10341=AXIS2_PLACEMENT_3D('',#16018,#12840,#12841);
#10342=AXIS2_PLACEMENT_3D('',#16019,#12842,#12843);
#10343=AXIS2_PLACEMENT_3D('',#16021,#12844,#12845);
#10344=AXIS2_PLACEMENT_3D('',#16024,#12847,#12848);
#10345=AXIS2_PLACEMENT_3D('',#16025,#12849,#12850);
#10346=AXIS2_PLACEMENT_3D('',#16027,#12851,#12852);
#10347=AXIS2_PLACEMENT_3D('',#16030,#12854,#12855);
#10348=AXIS2_PLACEMENT_3D('',#16031,#12856,#12857);
#10349=AXIS2_PLACEMENT_3D('',#16032,#12858,#12859);
#10350=AXIS2_PLACEMENT_3D('',#16033,#12860,#12861);
#10351=AXIS2_PLACEMENT_3D('',#16034,#12862,#12863);
#10352=AXIS2_PLACEMENT_3D('',#16035,#12864,#12865);
#10353=AXIS2_PLACEMENT_3D('',#16037,#12866,#12867);
#10354=AXIS2_PLACEMENT_3D('',#16040,#12869,#12870);
#10355=AXIS2_PLACEMENT_3D('',#16041,#12871,#12872);
#10356=AXIS2_PLACEMENT_3D('',#16042,#12873,#12874);
#10357=AXIS2_PLACEMENT_3D('',#16044,#12875,#12876);
#10358=AXIS2_PLACEMENT_3D('',#16047,#12878,#12879);
#10359=AXIS2_PLACEMENT_3D('',#16048,#12880,#12881);
#10360=AXIS2_PLACEMENT_3D('',#16050,#12882,#12883);
#10361=AXIS2_PLACEMENT_3D('',#16053,#12885,#12886);
#10362=AXIS2_PLACEMENT_3D('',#16054,#12887,#12888);
#10363=AXIS2_PLACEMENT_3D('',#16056,#12889,#12890);
#10364=AXIS2_PLACEMENT_3D('',#16059,#12892,#12893);
#10365=AXIS2_PLACEMENT_3D('',#16060,#12894,#12895);
#10366=AXIS2_PLACEMENT_3D('',#16062,#12896,#12897);
#10367=AXIS2_PLACEMENT_3D('',#16065,#12899,#12900);
#10368=AXIS2_PLACEMENT_3D('',#16066,#12901,#12902);
#10369=AXIS2_PLACEMENT_3D('',#16068,#12903,#12904);
#10370=AXIS2_PLACEMENT_3D('',#16071,#12906,#12907);
#10371=AXIS2_PLACEMENT_3D('',#16072,#12908,#12909);
#10372=AXIS2_PLACEMENT_3D('',#16081,#12914,#12915);
#10373=AXIS2_PLACEMENT_3D('',#16087,#12919,#12920);
#10374=AXIS2_PLACEMENT_3D('',#16093,#12924,#12925);
#10375=AXIS2_PLACEMENT_3D('',#16096,#12928,#12929);
#10376=AXIS2_PLACEMENT_3D('',#16097,#12930,#12931);
#10377=AXIS2_PLACEMENT_3D('',#16098,#12932,#12933);
#10378=AXIS2_PLACEMENT_3D('',#16099,#12934,#12935);
#10379=AXIS2_PLACEMENT_3D('',#16101,#12936,#12937);
#10380=AXIS2_PLACEMENT_3D('',#16104,#12939,#12940);
#10381=AXIS2_PLACEMENT_3D('',#16105,#12941,#12942);
#10382=AXIS2_PLACEMENT_3D('',#16107,#12943,#12944);
#10383=AXIS2_PLACEMENT_3D('',#16110,#12946,#12947);
#10384=AXIS2_PLACEMENT_3D('',#16111,#12948,#12949);
#10385=AXIS2_PLACEMENT_3D('',#16113,#12950,#12951);
#10386=AXIS2_PLACEMENT_3D('',#16116,#12953,#12954);
#10387=AXIS2_PLACEMENT_3D('',#16117,#12955,#12956);
#10388=AXIS2_PLACEMENT_3D('',#16119,#12957,#12958);
#10389=AXIS2_PLACEMENT_3D('',#16122,#12960,#12961);
#10390=AXIS2_PLACEMENT_3D('',#16123,#12962,#12963);
#10391=AXIS2_PLACEMENT_3D('',#16125,#12964,#12965);
#10392=AXIS2_PLACEMENT_3D('',#16128,#12967,#12968);
#10393=AXIS2_PLACEMENT_3D('',#16129,#12969,#12970);
#10394=AXIS2_PLACEMENT_3D('',#16138,#12975,#12976);
#10395=AXIS2_PLACEMENT_3D('',#16144,#12980,#12981);
#10396=AXIS2_PLACEMENT_3D('',#16150,#12985,#12986);
#10397=AXIS2_PLACEMENT_3D('',#16153,#12989,#12990);
#10398=AXIS2_PLACEMENT_3D('',#16154,#12991,#12992);
#10399=AXIS2_PLACEMENT_3D('',#16155,#12993,#12994);
#10400=AXIS2_PLACEMENT_3D('',#16156,#12995,#12996);
#10401=AXIS2_PLACEMENT_3D('',#16158,#12997,#12998);
#10402=AXIS2_PLACEMENT_3D('',#16161,#13000,#13001);
#10403=AXIS2_PLACEMENT_3D('',#16162,#13002,#13003);
#10404=AXIS2_PLACEMENT_3D('',#16164,#13004,#13005);
#10405=AXIS2_PLACEMENT_3D('',#16167,#13007,#13008);
#10406=AXIS2_PLACEMENT_3D('',#16168,#13009,#13010);
#10407=AXIS2_PLACEMENT_3D('',#16170,#13011,#13012);
#10408=AXIS2_PLACEMENT_3D('',#16173,#13014,#13015);
#10409=AXIS2_PLACEMENT_3D('',#16174,#13016,#13017);
#10410=AXIS2_PLACEMENT_3D('',#16176,#13018,#13019);
#10411=AXIS2_PLACEMENT_3D('',#16179,#13021,#13022);
#10412=AXIS2_PLACEMENT_3D('',#16180,#13023,#13024);
#10413=AXIS2_PLACEMENT_3D('',#16182,#13025,#13026);
#10414=AXIS2_PLACEMENT_3D('',#16185,#13028,#13029);
#10415=AXIS2_PLACEMENT_3D('',#16186,#13030,#13031);
#10416=AXIS2_PLACEMENT_3D('',#16195,#13036,#13037);
#10417=AXIS2_PLACEMENT_3D('',#16201,#13041,#13042);
#10418=AXIS2_PLACEMENT_3D('',#16207,#13046,#13047);
#10419=AXIS2_PLACEMENT_3D('',#16210,#13050,#13051);
#10420=AXIS2_PLACEMENT_3D('',#16211,#13052,#13053);
#10421=AXIS2_PLACEMENT_3D('',#16212,#13054,#13055);
#10422=AXIS2_PLACEMENT_3D('',#16213,#13056,#13057);
#10423=AXIS2_PLACEMENT_3D('',#16215,#13058,#13059);
#10424=AXIS2_PLACEMENT_3D('',#16218,#13061,#13062);
#10425=AXIS2_PLACEMENT_3D('',#16219,#13063,#13064);
#10426=AXIS2_PLACEMENT_3D('',#16220,#13065,#13066);
#10427=AXIS2_PLACEMENT_3D('',#16222,#13067,#13068);
#10428=AXIS2_PLACEMENT_3D('',#16224,#13069,#13070);
#10429=AXIS2_PLACEMENT_3D('',#16225,#13071,#13072);
#10430=AXIS2_PLACEMENT_3D('',#16227,#13073,#13074);
#10431=AXIS2_PLACEMENT_3D('',#16229,#13075,#13076);
#10432=AXIS2_PLACEMENT_3D('',#16230,#13077,#13078);
#10433=AXIS2_PLACEMENT_3D('',#16232,#13080,#13081);
#10434=AXIS2_PLACEMENT_3D('',#16235,#13083,#13084);
#10435=AXIS2_PLACEMENT_3D('',#16236,#13085,#13086);
#10436=AXIS2_PLACEMENT_3D('',#16238,#13087,#13088);
#10437=AXIS2_PLACEMENT_3D('',#16240,#13090,#13091);
#10438=AXIS2_PLACEMENT_3D('',#16241,#13092,#13093);
#10439=AXIS2_PLACEMENT_3D('',#16242,#13094,#13095);
#10440=AXIS2_PLACEMENT_3D('',#16243,#13096,#13097);
#10441=AXIS2_PLACEMENT_3D('',#16245,#13098,#13099);
#10442=AXIS2_PLACEMENT_3D('',#16248,#13101,#13102);
#10443=AXIS2_PLACEMENT_3D('',#16249,#13103,#13104);
#10444=AXIS2_PLACEMENT_3D('',#16251,#13105,#13106);
#10445=AXIS2_PLACEMENT_3D('',#16254,#13108,#13109);
#10446=AXIS2_PLACEMENT_3D('',#16255,#13110,#13111);
#10447=AXIS2_PLACEMENT_3D('',#16256,#13112,#13113);
#10448=AXIS2_PLACEMENT_3D('',#16257,#13114,#13115);
#10449=AXIS2_PLACEMENT_3D('',#16258,#13116,#13117);
#10450=AXIS2_PLACEMENT_3D('',#16260,#13118,#13119);
#10451=AXIS2_PLACEMENT_3D('',#16263,#13121,#13122);
#10452=AXIS2_PLACEMENT_3D('',#16264,#13123,#13124);
#10453=AXIS2_PLACEMENT_3D('',#16266,#13125,#13126);
#10454=AXIS2_PLACEMENT_3D('',#16269,#13128,#13129);
#10455=AXIS2_PLACEMENT_3D('',#16270,#13130,#13131);
#10456=AXIS2_PLACEMENT_3D('',#16271,#13132,#13133);
#10457=AXIS2_PLACEMENT_3D('',#16272,#13134,#13135);
#10458=AXIS2_PLACEMENT_3D('',#16273,#13136,#13137);
#10459=AXIS2_PLACEMENT_3D('',#16275,#13138,#13139);
#10460=AXIS2_PLACEMENT_3D('',#16278,#13141,#13142);
#10461=AXIS2_PLACEMENT_3D('',#16279,#13143,#13144);
#10462=AXIS2_PLACEMENT_3D('',#16281,#13145,#13146);
#10463=AXIS2_PLACEMENT_3D('',#16284,#13148,#13149);
#10464=AXIS2_PLACEMENT_3D('',#16285,#13150,#13151);
#10465=AXIS2_PLACEMENT_3D('',#16286,#13152,#13153);
#10466=AXIS2_PLACEMENT_3D('',#16287,#13154,#13155);
#10467=AXIS2_PLACEMENT_3D('',#16288,#13156,#13157);
#10468=AXIS2_PLACEMENT_3D('',#16289,#13158,#13159);
#10469=AXIS2_PLACEMENT_3D('',#16292,#13160,#13161);
#10470=AXIS2_PLACEMENT_3D('',#16298,#13165,#13166);
#10471=AXIS2_PLACEMENT_3D('',#16304,#13170,#13171);
#10472=AXIS2_PLACEMENT_3D('',#16306,#13172,#13173);
#10473=AXIS2_PLACEMENT_3D('',#16310,#13176,#13177);
#10474=AXIS2_PLACEMENT_3D('',#16313,#13180,#13181);
#10475=AXIS2_PLACEMENT_3D('',#16314,#13182,#13183);
#10476=AXIS2_PLACEMENT_3D('',#16316,#13184,#13185);
#10477=AXIS2_PLACEMENT_3D('',#16318,#13186,#13187);
#10478=AXIS2_PLACEMENT_3D('',#16319,#13188,#13189);
#10479=AXIS2_PLACEMENT_3D('',#16321,#13190,#13191);
#10480=AXIS2_PLACEMENT_3D('',#16323,#13193,#13194);
#10481=AXIS2_PLACEMENT_3D('',#16325,#13195,#13196);
#10482=AXIS2_PLACEMENT_3D('',#16326,#13197,#13198);
#10483=AXIS2_PLACEMENT_3D('',#16328,#13199,#13200);
#10484=AXIS2_PLACEMENT_3D('',#16330,#13202,#13203);
#10485=AXIS2_PLACEMENT_3D('',#16332,#13204,#13205);
#10486=AXIS2_PLACEMENT_3D('',#16333,#13206,#13207);
#10487=AXIS2_PLACEMENT_3D('',#16335,#13208,#13209);
#10488=AXIS2_PLACEMENT_3D('',#16337,#13211,#13212);
#10489=AXIS2_PLACEMENT_3D('',#16339,#13213,#13214);
#10490=AXIS2_PLACEMENT_3D('',#16340,#13215,#13216);
#10491=AXIS2_PLACEMENT_3D('',#16342,#13217,#13218);
#10492=AXIS2_PLACEMENT_3D('',#16344,#13220,#13221);
#10493=AXIS2_PLACEMENT_3D('',#16346,#13222,#13223);
#10494=AXIS2_PLACEMENT_3D('',#16347,#13224,#13225);
#10495=AXIS2_PLACEMENT_3D('',#16349,#13226,#13227);
#10496=AXIS2_PLACEMENT_3D('',#16351,#13229,#13230);
#10497=AXIS2_PLACEMENT_3D('',#16353,#13231,#13232);
#10498=AXIS2_PLACEMENT_3D('',#16354,#13233,#13234);
#10499=AXIS2_PLACEMENT_3D('',#16356,#13236,#13237);
#10500=AXIS2_PLACEMENT_3D('',#16357,#13238,#13239);
#10501=AXIS2_PLACEMENT_3D('',#16360,#13240,#13241);
#10502=AXIS2_PLACEMENT_3D('',#16364,#13243,#13244);
#10503=AXIS2_PLACEMENT_3D('',#16366,#13246,#13247);
#10504=AXIS2_PLACEMENT_3D('',#16372,#13251,#13252);
#10505=AXIS2_PLACEMENT_3D('',#16374,#13253,#13254);
#10506=AXIS2_PLACEMENT_3D('',#16376,#13255,#13256);
#10507=AXIS2_PLACEMENT_3D('',#16378,#13258,#13259);
#10508=AXIS2_PLACEMENT_3D('',#16381,#13262,#13263);
#10509=AXIS2_PLACEMENT_3D('',#16383,#13264,#13265);
#10510=AXIS2_PLACEMENT_3D('',#16385,#13266,#13267);
#10511=AXIS2_PLACEMENT_3D('',#16386,#13268,#13269);
#10512=AXIS2_PLACEMENT_3D('',#16388,#13270,#13271);
#10513=AXIS2_PLACEMENT_3D('',#16390,#13273,#13274);
#10514=AXIS2_PLACEMENT_3D('',#16392,#13275,#13276);
#10515=AXIS2_PLACEMENT_3D('',#16393,#13277,#13278);
#10516=AXIS2_PLACEMENT_3D('',#16395,#13280,#13281);
#10517=AXIS2_PLACEMENT_3D('',#16396,#13282,#13283);
#10518=AXIS2_PLACEMENT_3D('',#16397,#13284,#13285);
#10519=AXIS2_PLACEMENT_3D('',#16398,#13286,#13287);
#10520=AXIS2_PLACEMENT_3D('',#16407,#13292,#13293);
#10521=AXIS2_PLACEMENT_3D('',#16413,#13297,#13298);
#10522=AXIS2_PLACEMENT_3D('',#16419,#13302,#13303);
#10523=AXIS2_PLACEMENT_3D('',#16425,#13307,#13308);
#10524=AXIS2_PLACEMENT_3D('',#16431,#13312,#13313);
#10525=AXIS2_PLACEMENT_3D('',#16434,#13316,#13317);
#10526=AXIS2_PLACEMENT_3D('',#16435,#13318,#13319);
#10527=AXIS2_PLACEMENT_3D('',#16436,#13320,#13321);
#10528=AXIS2_PLACEMENT_3D('',#16438,#13322,#13323);
#10529=AXIS2_PLACEMENT_3D('',#16439,#13324,#13325);
#10530=AXIS2_PLACEMENT_3D('',#16441,#13326,#13327);
#10531=AXIS2_PLACEMENT_3D('',#16442,#13328,#13329);
#10532=AXIS2_PLACEMENT_3D('',#16444,#13330,#13331);
#10533=AXIS2_PLACEMENT_3D('',#16446,#13333,#13334);
#10534=AXIS2_PLACEMENT_3D('',#16448,#13335,#13336);
#10535=AXIS2_PLACEMENT_3D('',#16450,#13338,#13339);
#10536=AXIS2_PLACEMENT_3D('',#16452,#13340,#13341);
#10537=AXIS2_PLACEMENT_3D('',#16454,#13343,#13344);
#10538=AXIS2_PLACEMENT_3D('',#16456,#13345,#13346);
#10539=AXIS2_PLACEMENT_3D('',#16457,#13347,#13348);
#10540=AXIS2_PLACEMENT_3D('',#16459,#13349,#13350);
#10541=AXIS2_PLACEMENT_3D('',#16461,#13352,#13353);
#10542=AXIS2_PLACEMENT_3D('',#16463,#13355,#13356);
#10543=AXIS2_PLACEMENT_3D('',#16464,#13357,#13358);
#10544=AXIS2_PLACEMENT_3D('',#16465,#13359,#13360);
#10545=AXIS2_PLACEMENT_3D('',#16466,#13361,#13362);
#10546=AXIS2_PLACEMENT_3D('',#16467,#13363,#13364);
#10547=AXIS2_PLACEMENT_3D('',#16468,#13365,#13366);
#10548=AXIS2_PLACEMENT_3D('',#16469,#13367,#13368);
#10549=AXIS2_PLACEMENT_3D('',#16470,#13369,#13370);
#10550=AXIS2_PLACEMENT_3D('',#16471,#13371,#13372);
#10551=AXIS2_PLACEMENT_3D('',#16472,#13373,#13374);
#10552=AXIS2_PLACEMENT_3D('',#16473,#13375,#13376);
#10553=AXIS2_PLACEMENT_3D('',#16474,#13377,#13378);
#10554=AXIS2_PLACEMENT_3D('',#16475,#13379,#13380);
#10555=AXIS2_PLACEMENT_3D('',#16476,#13381,#13382);
#10556=AXIS2_PLACEMENT_3D('',#16477,#13383,#13384);
#10557=AXIS2_PLACEMENT_3D('',#16478,#13385,#13386);
#10558=AXIS2_PLACEMENT_3D('',#16479,#13387,#13388);
#10559=AXIS2_PLACEMENT_3D('',#16480,#13389,#13390);
#10560=AXIS2_PLACEMENT_3D('',#16481,#13391,#13392);
#10561=AXIS2_PLACEMENT_3D('',#16482,#13393,#13394);
#10562=AXIS2_PLACEMENT_3D('',#16483,#13395,#13396);
#10563=AXIS2_PLACEMENT_3D('',#16484,#13397,#13398);
#10564=AXIS2_PLACEMENT_3D('',#16485,#13399,#13400);
#10565=AXIS2_PLACEMENT_3D('',#16486,#13401,#13402);
#10566=AXIS2_PLACEMENT_3D('',#16487,#13403,#13404);
#10567=AXIS2_PLACEMENT_3D('',#16488,#13405,#13406);
#10568=AXIS2_PLACEMENT_3D('',#16489,#13407,#13408);
#10569=AXIS2_PLACEMENT_3D('',#16490,#13409,#13410);
#10570=AXIS2_PLACEMENT_3D('',#16491,#13411,#13412);
#10571=AXIS2_PLACEMENT_3D('',#16492,#13413,#13414);
#10572=AXIS2_PLACEMENT_3D('',#16493,#13415,#13416);
#10573=AXIS2_PLACEMENT_3D('',#16494,#13417,#13418);
#10574=AXIS2_PLACEMENT_3D('',#16495,#13419,#13420);
#10575=AXIS2_PLACEMENT_3D('',#16496,#13421,#13422);
#10576=AXIS2_PLACEMENT_3D('',#16497,#13423,#13424);
#10577=AXIS2_PLACEMENT_3D('',#16498,#13425,#13426);
#10578=AXIS2_PLACEMENT_3D('',#16499,#13427,#13428);
#10579=AXIS2_PLACEMENT_3D('',#16500,#13429,#13430);
#10580=AXIS2_PLACEMENT_3D('',#16501,#13431,#13432);
#10581=AXIS2_PLACEMENT_3D('',#16502,#13433,#13434);
#10582=AXIS2_PLACEMENT_3D('',#16503,#13435,#13436);
#10583=AXIS2_PLACEMENT_3D('',#16504,#13437,#13438);
#10584=AXIS2_PLACEMENT_3D('',#16505,#13439,#13440);
#10585=AXIS2_PLACEMENT_3D('',#16506,#13441,#13442);
#10586=AXIS2_PLACEMENT_3D('',#16507,#13443,#13444);
#10587=AXIS2_PLACEMENT_3D('',#16508,#13445,#13446);
#10588=AXIS2_PLACEMENT_3D('',#16509,#13447,#13448);
#10589=AXIS2_PLACEMENT_3D('',#16510,#13449,#13450);
#10590=AXIS2_PLACEMENT_3D('',#16511,#13451,#13452);
#10591=AXIS2_PLACEMENT_3D('',#16512,#13453,#13454);
#10592=AXIS2_PLACEMENT_3D('',#16513,#13455,#13456);
#10593=AXIS2_PLACEMENT_3D('',#16514,#13457,#13458);
#10594=AXIS2_PLACEMENT_3D('',#16515,#13459,#13460);
#10595=AXIS2_PLACEMENT_3D('',#16516,#13461,#13462);
#10596=AXIS2_PLACEMENT_3D('',#16517,#13463,#13464);
#10597=AXIS2_PLACEMENT_3D('',#16518,#13465,#13466);
#10598=AXIS2_PLACEMENT_3D('',#16519,#13467,#13468);
#10599=AXIS2_PLACEMENT_3D('',#16520,#13469,#13470);
#10600=AXIS2_PLACEMENT_3D('',#16521,#13471,#13472);
#10601=AXIS2_PLACEMENT_3D('',#16522,#13473,#13474);
#10602=AXIS2_PLACEMENT_3D('',#16523,#13475,#13476);
#10603=AXIS2_PLACEMENT_3D('',#16524,#13477,#13478);
#10604=AXIS2_PLACEMENT_3D('',#16525,#13479,#13480);
#10605=AXIS2_PLACEMENT_3D('',#16526,#13481,#13482);
#10606=AXIS2_PLACEMENT_3D('',#16527,#13483,#13484);
#10607=AXIS2_PLACEMENT_3D('',#16528,#13485,#13486);
#10608=AXIS2_PLACEMENT_3D('',#16529,#13487,#13488);
#10609=AXIS2_PLACEMENT_3D('',#16530,#13489,#13490);
#10610=AXIS2_PLACEMENT_3D('',#16531,#13491,#13492);
#10611=AXIS2_PLACEMENT_3D('',#16532,#13493,#13494);
#10612=AXIS2_PLACEMENT_3D('',#16533,#13495,#13496);
#10613=AXIS2_PLACEMENT_3D('',#16534,#13497,#13498);
#10614=AXIS2_PLACEMENT_3D('',#16535,#13499,#13500);
#10615=AXIS2_PLACEMENT_3D('',#16536,#13501,#13502);
#10616=AXIS2_PLACEMENT_3D('',#16537,#13503,#13504);
#10617=AXIS2_PLACEMENT_3D('',#16538,#13505,#13506);
#10618=AXIS2_PLACEMENT_3D('',#16539,#13507,#13508);
#10619=AXIS2_PLACEMENT_3D('',#16540,#13509,#13510);
#10620=AXIS2_PLACEMENT_3D('',#16541,#13511,#13512);
#10621=AXIS2_PLACEMENT_3D('',#16542,#13513,#13514);
#10622=AXIS2_PLACEMENT_3D('',#16543,#13515,#13516);
#10623=AXIS2_PLACEMENT_3D('',#16544,#13517,#13518);
#10624=AXIS2_PLACEMENT_3D('',#16545,#13519,#13520);
#10625=AXIS2_PLACEMENT_3D('',#16546,#13521,#13522);
#10626=AXIS2_PLACEMENT_3D('',#16547,#13523,#13524);
#10627=AXIS2_PLACEMENT_3D('',#16548,#13525,#13526);
#10628=AXIS2_PLACEMENT_3D('',#16549,#13527,#13528);
#10629=AXIS2_PLACEMENT_3D('',#16550,#13529,#13530);
#10630=DIRECTION('axis',(0.,0.,1.));
#10631=DIRECTION('refdir',(1.,0.,0.));
#10632=DIRECTION('axis',(0.,0.,1.));
#10633=DIRECTION('refdir',(1.,0.,0.));
#10634=DIRECTION('axis',(0.,0.,1.));
#10635=DIRECTION('refdir',(1.,0.,0.));
#10636=DIRECTION('center_axis',(0.,0.,1.));
#10637=DIRECTION('ref_axis',(1.,0.,0.));
#10638=DIRECTION('center_axis',(0.,0.,1.));
#10639=DIRECTION('ref_axis',(1.,0.,0.));
#10640=DIRECTION('',(0.,0.,1.));
#10641=DIRECTION('center_axis',(0.,0.,-1.));
#10642=DIRECTION('ref_axis',(1.,0.,0.));
#10643=DIRECTION('center_axis',(0.,0.,1.));
#10644=DIRECTION('ref_axis',(1.,0.,0.));
#10645=DIRECTION('center_axis',(0.,0.,1.));
#10646=DIRECTION('ref_axis',(1.,0.,0.));
#10647=DIRECTION('',(0.,0.,1.));
#10648=DIRECTION('center_axis',(0.,0.,-1.));
#10649=DIRECTION('ref_axis',(1.,0.,0.));
#10650=DIRECTION('center_axis',(0.,0.,1.));
#10651=DIRECTION('ref_axis',(1.,0.,0.));
#10652=DIRECTION('center_axis',(0.,0.,1.));
#10653=DIRECTION('ref_axis',(1.,0.,0.));
#10654=DIRECTION('',(0.,0.,1.));
#10655=DIRECTION('center_axis',(0.,0.,-1.));
#10656=DIRECTION('ref_axis',(1.,0.,0.));
#10657=DIRECTION('center_axis',(0.,0.,1.));
#10658=DIRECTION('ref_axis',(1.,0.,0.));
#10659=DIRECTION('center_axis',(0.,0.,1.));
#10660=DIRECTION('ref_axis',(1.,0.,0.));
#10661=DIRECTION('',(0.,0.,1.));
#10662=DIRECTION('center_axis',(0.,0.,-1.));
#10663=DIRECTION('ref_axis',(1.,0.,0.));
#10664=DIRECTION('center_axis',(0.,0.,1.));
#10665=DIRECTION('ref_axis',(1.,0.,0.));
#10666=DIRECTION('center_axis',(0.,0.,1.));
#10667=DIRECTION('ref_axis',(1.,0.,0.));
#10668=DIRECTION('',(0.,0.,1.));
#10669=DIRECTION('center_axis',(0.,0.,-1.));
#10670=DIRECTION('ref_axis',(1.,0.,0.));
#10671=DIRECTION('center_axis',(0.,0.,1.));
#10672=DIRECTION('ref_axis',(1.,0.,0.));
#10673=DIRECTION('center_axis',(0.,0.,1.));
#10674=DIRECTION('ref_axis',(1.,0.,0.));
#10675=DIRECTION('',(0.,0.,1.));
#10676=DIRECTION('center_axis',(0.,0.,-1.));
#10677=DIRECTION('ref_axis',(1.,0.,0.));
#10678=DIRECTION('center_axis',(0.,0.,1.));
#10679=DIRECTION('ref_axis',(1.,0.,0.));
#10680=DIRECTION('center_axis',(0.,0.,1.));
#10681=DIRECTION('ref_axis',(1.,0.,0.));
#10682=DIRECTION('',(0.,0.,1.));
#10683=DIRECTION('center_axis',(0.,0.,-1.));
#10684=DIRECTION('ref_axis',(1.,0.,0.));
#10685=DIRECTION('center_axis',(0.,0.,1.));
#10686=DIRECTION('ref_axis',(1.,0.,0.));
#10687=DIRECTION('center_axis',(0.,0.,1.));
#10688=DIRECTION('ref_axis',(1.,0.,0.));
#10689=DIRECTION('',(0.,0.,1.));
#10690=DIRECTION('center_axis',(0.,0.,-1.));
#10691=DIRECTION('ref_axis',(1.,0.,0.));
#10692=DIRECTION('center_axis',(0.,0.,1.));
#10693=DIRECTION('ref_axis',(1.,0.,0.));
#10694=DIRECTION('center_axis',(0.,0.,1.));
#10695=DIRECTION('ref_axis',(1.,0.,0.));
#10696=DIRECTION('',(0.,0.,1.));
#10697=DIRECTION('center_axis',(0.,0.,-1.));
#10698=DIRECTION('ref_axis',(1.,0.,0.));
#10699=DIRECTION('center_axis',(0.,0.,1.));
#10700=DIRECTION('ref_axis',(1.,0.,0.));
#10701=DIRECTION('center_axis',(0.,0.,1.));
#10702=DIRECTION('ref_axis',(1.,0.,0.));
#10703=DIRECTION('',(0.,0.,1.));
#10704=DIRECTION('center_axis',(0.,0.,-1.));
#10705=DIRECTION('ref_axis',(1.,0.,0.));
#10706=DIRECTION('center_axis',(0.,0.,1.));
#10707=DIRECTION('ref_axis',(1.,0.,0.));
#10708=DIRECTION('center_axis',(0.,0.,1.));
#10709=DIRECTION('ref_axis',(1.,0.,0.));
#10710=DIRECTION('',(0.,0.,1.));
#10711=DIRECTION('center_axis',(0.,0.,-1.));
#10712=DIRECTION('ref_axis',(1.,0.,0.));
#10713=DIRECTION('center_axis',(0.,0.,1.));
#10714=DIRECTION('ref_axis',(1.,0.,0.));
#10715=DIRECTION('center_axis',(0.,0.,1.));
#10716=DIRECTION('ref_axis',(1.,0.,0.));
#10717=DIRECTION('',(0.,0.,1.));
#10718=DIRECTION('center_axis',(0.,0.,-1.));
#10719=DIRECTION('ref_axis',(1.,0.,0.));
#10720=DIRECTION('center_axis',(0.,1.,0.));
#10721=DIRECTION('ref_axis',(-1.,0.,0.));
#10722=DIRECTION('',(-1.,0.,0.));
#10723=DIRECTION('',(0.,0.,1.));
#10724=DIRECTION('',(-1.,0.,0.));
#10725=DIRECTION('',(0.,0.,1.));
#10726=DIRECTION('center_axis',(1.,0.,0.));
#10727=DIRECTION('ref_axis',(0.,1.,0.));
#10728=DIRECTION('',(0.,1.,0.));
#10729=DIRECTION('',(0.,1.,0.));
#10730=DIRECTION('',(0.,0.,1.));
#10731=DIRECTION('center_axis',(0.,-1.,0.));
#10732=DIRECTION('ref_axis',(1.,0.,0.));
#10733=DIRECTION('',(1.,0.,0.));
#10734=DIRECTION('',(1.,0.,0.));
#10735=DIRECTION('',(0.,0.,1.));
#10736=DIRECTION('center_axis',(-1.,0.,0.));
#10737=DIRECTION('ref_axis',(0.,-1.,0.));
#10738=DIRECTION('',(0.,-1.,0.));
#10739=DIRECTION('',(0.,-1.,0.));
#10740=DIRECTION('center_axis',(0.,0.,1.));
#10741=DIRECTION('ref_axis',(1.,0.,0.));
#10742=DIRECTION('center_axis',(0.,0.,1.));
#10743=DIRECTION('ref_axis',(1.,0.,0.));
#10744=DIRECTION('axis',(0.,0.,1.));
#10745=DIRECTION('refdir',(1.,0.,0.));
#10746=DIRECTION('center_axis',(0.,1.,0.));
#10747=DIRECTION('ref_axis',(-1.,0.,0.));
#10748=DIRECTION('',(-1.,0.,0.));
#10749=DIRECTION('',(0.,0.,1.));
#10750=DIRECTION('',(-1.,0.,0.));
#10751=DIRECTION('',(0.,0.,1.));
#10752=DIRECTION('center_axis',(1.,0.,0.));
#10753=DIRECTION('ref_axis',(0.,1.,0.));
#10754=DIRECTION('',(0.,1.,0.));
#10755=DIRECTION('',(0.,1.,0.));
#10756=DIRECTION('',(0.,0.,1.));
#10757=DIRECTION('center_axis',(0.,-1.,0.));
#10758=DIRECTION('ref_axis',(1.,0.,0.));
#10759=DIRECTION('',(1.,0.,0.));
#10760=DIRECTION('',(1.,0.,0.));
#10761=DIRECTION('',(0.,0.,1.));
#10762=DIRECTION('center_axis',(-1.,0.,0.));
#10763=DIRECTION('ref_axis',(0.,-1.,0.));
#10764=DIRECTION('',(0.,-1.,0.));
#10765=DIRECTION('',(0.,-1.,0.));
#10766=DIRECTION('center_axis',(0.,0.,1.));
#10767=DIRECTION('ref_axis',(1.,0.,0.));
#10768=DIRECTION('center_axis',(0.,0.,1.));
#10769=DIRECTION('ref_axis',(1.,0.,0.));
#10770=DIRECTION('axis',(0.,0.,1.));
#10771=DIRECTION('refdir',(1.,0.,0.));
#10772=DIRECTION('center_axis',(0.,1.,0.));
#10773=DIRECTION('ref_axis',(-1.,0.,0.));
#10774=DIRECTION('',(-1.,0.,0.));
#10775=DIRECTION('',(0.,0.,1.));
#10776=DIRECTION('',(-1.,0.,0.));
#10777=DIRECTION('',(0.,0.,1.));
#10778=DIRECTION('center_axis',(1.,0.,0.));
#10779=DIRECTION('ref_axis',(0.,1.,0.));
#10780=DIRECTION('',(0.,1.,0.));
#10781=DIRECTION('',(0.,1.,0.));
#10782=DIRECTION('',(0.,0.,1.));
#10783=DIRECTION('center_axis',(0.,-1.,0.));
#10784=DIRECTION('ref_axis',(1.,0.,0.));
#10785=DIRECTION('',(1.,0.,0.));
#10786=DIRECTION('',(1.,0.,0.));
#10787=DIRECTION('',(0.,0.,1.));
#10788=DIRECTION('center_axis',(-1.,0.,0.));
#10789=DIRECTION('ref_axis',(0.,-1.,0.));
#10790=DIRECTION('',(0.,-1.,0.));
#10791=DIRECTION('',(0.,-1.,0.));
#10792=DIRECTION('center_axis',(0.,0.,1.));
#10793=DIRECTION('ref_axis',(1.,0.,0.));
#10794=DIRECTION('center_axis',(0.,0.,1.));
#10795=DIRECTION('ref_axis',(1.,0.,0.));
#10796=DIRECTION('axis',(0.,0.,1.));
#10797=DIRECTION('refdir',(1.,0.,0.));
#10798=DIRECTION('center_axis',(1.,0.,0.));
#10799=DIRECTION('ref_axis',(0.,0.,-1.));
#10800=DIRECTION('',(1.,0.,0.));
#10801=DIRECTION('center_axis',(0.,0.,1.));
#10802=DIRECTION('ref_axis',(1.,0.,0.));
#10803=DIRECTION('center_axis',(0.,0.,1.));
#10804=DIRECTION('ref_axis',(1.,0.,0.));
#10805=DIRECTION('',(0.,0.,1.));
#10806=DIRECTION('center_axis',(0.,0.,-1.));
#10807=DIRECTION('ref_axis',(1.,0.,0.));
#10808=DIRECTION('center_axis',(0.,0.,1.));
#10809=DIRECTION('ref_axis',(1.,0.,0.));
#10810=DIRECTION('center_axis',(0.,0.,1.));
#10811=DIRECTION('ref_axis',(1.,0.,0.));
#10812=DIRECTION('center_axis',(0.,0.,1.));
#10813=DIRECTION('ref_axis',(1.,0.,0.));
#10814=DIRECTION('',(0.,0.,1.));
#10815=DIRECTION('center_axis',(0.,0.,-1.));
#10816=DIRECTION('ref_axis',(1.,0.,0.));
#10817=DIRECTION('center_axis',(0.,0.,1.));
#10818=DIRECTION('ref_axis',(1.,0.,0.));
#10819=DIRECTION('center_axis',(0.,0.,1.));
#10820=DIRECTION('ref_axis',(1.,0.,0.));
#10821=DIRECTION('center_axis',(0.,0.,1.));
#10822=DIRECTION('ref_axis',(1.,0.,0.));
#10823=DIRECTION('',(0.,0.,1.));
#10824=DIRECTION('center_axis',(0.,0.,-1.));
#10825=DIRECTION('ref_axis',(1.,0.,0.));
#10826=DIRECTION('center_axis',(0.,0.,1.));
#10827=DIRECTION('ref_axis',(1.,0.,0.));
#10828=DIRECTION('center_axis',(0.,0.,1.));
#10829=DIRECTION('ref_axis',(1.,0.,0.));
#10830=DIRECTION('center_axis',(0.,0.,1.));
#10831=DIRECTION('ref_axis',(1.,0.,0.));
#10832=DIRECTION('',(0.,0.,1.));
#10833=DIRECTION('center_axis',(0.,0.,-1.));
#10834=DIRECTION('ref_axis',(1.,0.,0.));
#10835=DIRECTION('center_axis',(0.,0.,1.));
#10836=DIRECTION('ref_axis',(1.,0.,0.));
#10837=DIRECTION('center_axis',(0.,0.,1.));
#10838=DIRECTION('ref_axis',(1.,0.,0.));
#10839=DIRECTION('center_axis',(0.,0.,1.));
#10840=DIRECTION('ref_axis',(1.,0.,0.));
#10841=DIRECTION('center_axis',(0.,0.,1.));
#10842=DIRECTION('ref_axis',(1.,0.,0.));
#10843=DIRECTION('center_axis',(0.,0.,1.));
#10844=DIRECTION('ref_axis',(1.,0.,0.));
#10845=DIRECTION('',(0.,0.,1.));
#10846=DIRECTION('center_axis',(0.,0.,1.));
#10847=DIRECTION('ref_axis',(1.,0.,0.));
#10848=DIRECTION('',(0.,0.,-1.));
#10849=DIRECTION('center_axis',(0.,0.,1.));
#10850=DIRECTION('ref_axis',(1.,0.,0.));
#10851=DIRECTION('',(0.,0.,-1.));
#10852=DIRECTION('center_axis',(0.,0.,1.));
#10853=DIRECTION('ref_axis',(1.,0.,0.));
#10854=DIRECTION('',(0.,0.,1.));
#10855=DIRECTION('center_axis',(0.,0.,1.));
#10856=DIRECTION('ref_axis',(1.,0.,0.));
#10857=DIRECTION('center_axis',(0.,0.,1.));
#10858=DIRECTION('ref_axis',(1.,0.,0.));
#10859=DIRECTION('center_axis',(0.,0.,1.));
#10860=DIRECTION('ref_axis',(1.,0.,0.));
#10861=DIRECTION('center_axis',(0.,0.,1.));
#10862=DIRECTION('ref_axis',(-0.707106781186548,-0.707106781186547,0.));
#10863=DIRECTION('',(0.,0.,-1.));
#10864=DIRECTION('center_axis',(0.,0.,1.));
#10865=DIRECTION('ref_axis',(1.,0.,0.));
#10866=DIRECTION('',(0.,0.,1.));
#10867=DIRECTION('center_axis',(0.,0.,1.));
#10868=DIRECTION('ref_axis',(1.,0.,0.));
#10869=DIRECTION('center_axis',(0.,0.,1.));
#10870=DIRECTION('ref_axis',(1.,0.,0.));
#10871=DIRECTION('center_axis',(0.,0.,1.));
#10872=DIRECTION('ref_axis',(1.,0.,0.));
#10873=DIRECTION('center_axis',(0.,0.,1.));
#10874=DIRECTION('ref_axis',(-0.707106781186547,0.707106781186548,0.));
#10875=DIRECTION('',(0.,0.,-1.));
#10876=DIRECTION('center_axis',(0.,0.,1.));
#10877=DIRECTION('ref_axis',(1.,0.,0.));
#10878=DIRECTION('',(0.,0.,1.));
#10879=DIRECTION('center_axis',(0.,0.,1.));
#10880=DIRECTION('ref_axis',(1.,0.,0.));
#10881=DIRECTION('center_axis',(0.,0.,1.));
#10882=DIRECTION('ref_axis',(1.,0.,0.));
#10883=DIRECTION('center_axis',(0.,0.,1.));
#10884=DIRECTION('ref_axis',(1.,0.,0.));
#10885=DIRECTION('center_axis',(0.,0.,1.));
#10886=DIRECTION('ref_axis',(1.,0.,0.));
#10887=DIRECTION('center_axis',(0.,0.,1.));
#10888=DIRECTION('ref_axis',(1.,0.,0.));
#10889=DIRECTION('',(0.,0.,-1.));
#10890=DIRECTION('center_axis',(0.,0.,1.));
#10891=DIRECTION('ref_axis',(1.,0.,0.));
#10892=DIRECTION('center_axis',(0.,0.,1.));
#10893=DIRECTION('ref_axis',(1.,0.,0.));
#10894=DIRECTION('center_axis',(0.,0.,1.));
#10895=DIRECTION('ref_axis',(1.,0.,0.));
#10896=DIRECTION('center_axis',(0.,0.,1.));
#10897=DIRECTION('ref_axis',(1.,0.,0.));
#10898=DIRECTION('center_axis',(0.,0.,1.));
#10899=DIRECTION('ref_axis',(1.,0.,0.));
#10900=DIRECTION('center_axis',(0.,0.,1.));
#10901=DIRECTION('ref_axis',(1.,0.,0.));
#10902=DIRECTION('center_axis',(0.,0.,1.));
#10903=DIRECTION('ref_axis',(1.,0.,0.));
#10904=DIRECTION('center_axis',(0.,0.,-1.));
#10905=DIRECTION('ref_axis',(1.,0.,0.));
#10906=DIRECTION('center_axis',(0.,0.,-1.));
#10907=DIRECTION('ref_axis',(1.,0.,0.));
#10908=DIRECTION('center_axis',(0.,0.,-1.));
#10909=DIRECTION('ref_axis',(1.,0.,0.));
#10910=DIRECTION('center_axis',(0.,0.,-1.));
#10911=DIRECTION('ref_axis',(1.,0.,0.));
#10912=DIRECTION('center_axis',(0.,0.,1.));
#10913=DIRECTION('ref_axis',(1.,0.,0.));
#10914=DIRECTION('center_axis',(0.,0.,1.));
#10915=DIRECTION('ref_axis',(1.,0.,0.));
#10916=DIRECTION('',(0.,0.,1.));
#10917=DIRECTION('center_axis',(0.,0.,1.));
#10918=DIRECTION('ref_axis',(1.,0.,0.));
#10919=DIRECTION('center_axis',(0.,0.,1.));
#10920=DIRECTION('ref_axis',(1.,0.,0.));
#10921=DIRECTION('',(0.,0.,1.));
#10922=DIRECTION('center_axis',(0.,0.,1.));
#10923=DIRECTION('ref_axis',(1.,0.,0.));
#10924=DIRECTION('center_axis',(0.,0.,1.));
#10925=DIRECTION('ref_axis',(1.,0.,0.));
#10926=DIRECTION('',(0.,0.,1.));
#10927=DIRECTION('center_axis',(0.,0.,1.));
#10928=DIRECTION('ref_axis',(1.,0.,0.));
#10929=DIRECTION('center_axis',(0.,0.,1.));
#10930=DIRECTION('ref_axis',(1.,0.,0.));
#10931=DIRECTION('',(0.,0.,1.));
#10932=DIRECTION('center_axis',(0.,0.,1.));
#10933=DIRECTION('ref_axis',(1.,0.,0.));
#10934=DIRECTION('center_axis',(0.,0.,1.));
#10935=DIRECTION('ref_axis',(1.,0.,0.));
#10936=DIRECTION('',(0.,0.,1.));
#10937=DIRECTION('center_axis',(0.,0.,-1.));
#10938=DIRECTION('ref_axis',(1.,0.,0.));
#10939=DIRECTION('center_axis',(0.,0.,1.));
#10940=DIRECTION('ref_axis',(1.,0.,0.));
#10941=DIRECTION('center_axis',(0.,0.,1.));
#10942=DIRECTION('ref_axis',(1.,0.,0.));
#10943=DIRECTION('center_axis',(0.,0.,1.));
#10944=DIRECTION('ref_axis',(1.,0.,0.));
#10945=DIRECTION('',(0.,0.,-1.));
#10946=DIRECTION('center_axis',(0.,0.,1.));
#10947=DIRECTION('ref_axis',(1.,0.,0.));
#10948=DIRECTION('center_axis',(0.,0.,1.));
#10949=DIRECTION('ref_axis',(1.,0.,0.));
#10950=DIRECTION('',(0.,0.,-1.));
#10951=DIRECTION('center_axis',(0.,0.,-1.));
#10952=DIRECTION('ref_axis',(1.,0.,0.));
#10953=DIRECTION('center_axis',(0.,0.,1.));
#10954=DIRECTION('ref_axis',(1.,0.,0.));
#10955=DIRECTION('center_axis',(0.,0.,1.));
#10956=DIRECTION('ref_axis',(1.,0.,0.));
#10957=DIRECTION('axis',(0.,0.,1.));
#10958=DIRECTION('refdir',(1.,0.,0.));
#10959=DIRECTION('center_axis',(0.,0.,1.));
#10960=DIRECTION('ref_axis',(1.,0.,0.));
#10961=DIRECTION('center_axis',(0.,0.,1.));
#10962=DIRECTION('ref_axis',(1.,0.,0.));
#10963=DIRECTION('',(0.,0.,1.));
#10964=DIRECTION('center_axis',(0.,0.,-1.));
#10965=DIRECTION('ref_axis',(1.,0.,0.));
#10966=DIRECTION('center_axis',(0.,0.,1.));
#10967=DIRECTION('ref_axis',(1.,0.,0.));
#10968=DIRECTION('center_axis',(0.,0.,1.));
#10969=DIRECTION('ref_axis',(1.,0.,0.));
#10970=DIRECTION('center_axis',(0.,0.,1.));
#10971=DIRECTION('ref_axis',(1.,0.,0.));
#10972=DIRECTION('center_axis',(0.,0.,1.));
#10973=DIRECTION('ref_axis',(1.,0.,0.));
#10974=DIRECTION('',(0.,0.,1.));
#10975=DIRECTION('center_axis',(0.,0.,-1.));
#10976=DIRECTION('ref_axis',(1.,0.,0.));
#10977=DIRECTION('center_axis',(0.,0.,1.));
#10978=DIRECTION('ref_axis',(1.,0.,0.));
#10979=DIRECTION('center_axis',(0.,0.,1.));
#10980=DIRECTION('ref_axis',(1.,0.,0.));
#10981=DIRECTION('center_axis',(0.,0.,1.));
#10982=DIRECTION('ref_axis',(1.,0.,0.));
#10983=DIRECTION('center_axis',(0.,0.,1.));
#10984=DIRECTION('ref_axis',(1.,0.,0.));
#10985=DIRECTION('',(0.,0.,1.));
#10986=DIRECTION('center_axis',(0.,0.,-1.));
#10987=DIRECTION('ref_axis',(1.,0.,0.));
#10988=DIRECTION('center_axis',(0.,0.,1.));
#10989=DIRECTION('ref_axis',(1.,0.,0.));
#10990=DIRECTION('center_axis',(0.,0.,1.));
#10991=DIRECTION('ref_axis',(1.,0.,0.));
#10992=DIRECTION('center_axis',(0.,0.,1.));
#10993=DIRECTION('ref_axis',(1.,0.,0.));
#10994=DIRECTION('center_axis',(0.,0.,1.));
#10995=DIRECTION('ref_axis',(1.,0.,0.));
#10996=DIRECTION('',(0.,0.,1.));
#10997=DIRECTION('center_axis',(0.,0.,-1.));
#10998=DIRECTION('ref_axis',(1.,0.,0.));
#10999=DIRECTION('center_axis',(0.,0.,1.));
#11000=DIRECTION('ref_axis',(1.,0.,0.));
#11001=DIRECTION('center_axis',(0.,0.,1.));
#11002=DIRECTION('ref_axis',(1.,0.,0.));
#11003=DIRECTION('center_axis',(0.,0.,1.));
#11004=DIRECTION('ref_axis',(1.,0.,0.));
#11005=DIRECTION('center_axis',(0.,0.,1.));
#11006=DIRECTION('ref_axis',(1.,0.,0.));
#11007=DIRECTION('',(0.,0.,1.));
#11008=DIRECTION('center_axis',(0.,0.,1.));
#11009=DIRECTION('ref_axis',(1.,0.,0.));
#11010=DIRECTION('center_axis',(0.,0.,1.));
#11011=DIRECTION('ref_axis',(1.,0.,0.));
#11012=DIRECTION('',(0.,0.,1.));
#11013=DIRECTION('center_axis',(0.,0.,1.));
#11014=DIRECTION('ref_axis',(1.,0.,0.));
#11015=DIRECTION('center_axis',(0.,0.,1.));
#11016=DIRECTION('ref_axis',(1.,0.,0.));
#11017=DIRECTION('',(0.,0.,1.));
#11018=DIRECTION('center_axis',(0.,0.,1.));
#11019=DIRECTION('ref_axis',(1.,0.,0.));
#11020=DIRECTION('center_axis',(0.,0.,1.));
#11021=DIRECTION('ref_axis',(1.,0.,0.));
#11022=DIRECTION('',(0.,0.,1.));
#11023=DIRECTION('center_axis',(0.,0.,1.));
#11024=DIRECTION('ref_axis',(1.,0.,0.));
#11025=DIRECTION('center_axis',(0.,0.,1.));
#11026=DIRECTION('ref_axis',(1.,0.,0.));
#11027=DIRECTION('',(0.,0.,-1.));
#11028=DIRECTION('center_axis',(0.,0.,1.));
#11029=DIRECTION('ref_axis',(1.,0.,0.));
#11030=DIRECTION('center_axis',(0.,0.,1.));
#11031=DIRECTION('ref_axis',(1.,0.,0.));
#11032=DIRECTION('center_axis',(0.,0.,-1.));
#11033=DIRECTION('ref_axis',(1.,0.,0.));
#11034=DIRECTION('center_axis',(0.,0.,1.));
#11035=DIRECTION('ref_axis',(1.,0.,0.));
#11036=DIRECTION('center_axis',(0.,0.,-1.));
#11037=DIRECTION('ref_axis',(1.,0.,0.));
#11038=DIRECTION('',(0.,0.,-1.));
#11039=DIRECTION('center_axis',(0.,0.,1.));
#11040=DIRECTION('ref_axis',(1.,0.,0.));
#11041=DIRECTION('center_axis',(0.,0.,1.));
#11042=DIRECTION('ref_axis',(1.,0.,0.));
#11043=DIRECTION('',(0.,0.,-1.));
#11044=DIRECTION('center_axis',(0.,0.,1.));
#11045=DIRECTION('ref_axis',(1.,0.,0.));
#11046=DIRECTION('center_axis',(0.,0.,1.));
#11047=DIRECTION('ref_axis',(1.,0.,0.));
#11048=DIRECTION('center_axis',(0.,0.,1.));
#11049=DIRECTION('ref_axis',(1.,0.,0.));
#11050=DIRECTION('axis',(0.,0.,1.));
#11051=DIRECTION('refdir',(1.,0.,0.));
#11052=DIRECTION('center_axis',(0.,0.,1.));
#11053=DIRECTION('ref_axis',(1.,0.,0.));
#11054=DIRECTION('',(0.,0.,1.));
#11055=DIRECTION('center_axis',(0.,0.,1.));
#11056=DIRECTION('ref_axis',(1.,0.,0.));
#11057=DIRECTION('',(0.,0.,1.));
#11058=DIRECTION('center_axis',(0.,0.,-1.));
#11059=DIRECTION('ref_axis',(1.,0.,0.));
#11060=DIRECTION('center_axis',(0.,0.,1.));
#11061=DIRECTION('ref_axis',(1.,0.,0.));
#11062=DIRECTION('',(0.,0.,1.));
#11063=DIRECTION('center_axis',(0.,0.,1.));
#11064=DIRECTION('ref_axis',(1.,0.,0.));
#11065=DIRECTION('',(0.,0.,1.));
#11066=DIRECTION('center_axis',(0.,0.,-1.));
#11067=DIRECTION('ref_axis',(1.,0.,0.));
#11068=DIRECTION('center_axis',(0.,0.,1.));
#11069=DIRECTION('ref_axis',(1.,0.,0.));
#11070=DIRECTION('',(1.,0.,0.));
#11071=DIRECTION('center_axis',(0.,0.,1.));
#11072=DIRECTION('ref_axis',(1.,0.,0.));
#11073=DIRECTION('center_axis',(0.,0.,1.));
#11074=DIRECTION('ref_axis',(1.,0.,0.));
#11075=DIRECTION('center_axis',(0.,0.,1.));
#11076=DIRECTION('ref_axis',(1.,0.,0.));
#11077=DIRECTION('',(0.,0.,1.));
#11078=DIRECTION('center_axis',(0.,0.,-1.));
#11079=DIRECTION('ref_axis',(1.,0.,0.));
#11080=DIRECTION('center_axis',(0.,0.,1.));
#11081=DIRECTION('ref_axis',(1.,0.,0.));
#11082=DIRECTION('',(-1.,0.,0.));
#11083=DIRECTION('center_axis',(0.,0.,1.));
#11084=DIRECTION('ref_axis',(1.,0.,0.));
#11085=DIRECTION('center_axis',(0.,0.,-1.));
#11086=DIRECTION('ref_axis',(1.,0.,0.));
#11087=DIRECTION('',(0.,0.,1.));
#11088=DIRECTION('center_axis',(0.,0.,1.));
#11089=DIRECTION('ref_axis',(1.,0.,0.));
#11090=DIRECTION('center_axis',(0.,0.,1.));
#11091=DIRECTION('ref_axis',(1.,0.,0.));
#11092=DIRECTION('center_axis',(0.,0.,1.));
#11093=DIRECTION('ref_axis',(1.,0.,0.));
#11094=DIRECTION('center_axis',(0.,0.,1.));
#11095=DIRECTION('ref_axis',(1.,0.,0.));
#11096=DIRECTION('center_axis',(0.,0.,-1.));
#11097=DIRECTION('ref_axis',(1.,0.,0.));
#11098=DIRECTION('',(0.,0.,1.));
#11099=DIRECTION('center_axis',(0.,0.,1.));
#11100=DIRECTION('ref_axis',(1.,0.,0.));
#11101=DIRECTION('center_axis',(0.,0.,1.));
#11102=DIRECTION('ref_axis',(1.,0.,0.));
#11103=DIRECTION('center_axis',(0.,0.,1.));
#11104=DIRECTION('ref_axis',(1.,0.,0.));
#11105=DIRECTION('center_axis',(0.,0.,1.));
#11106=DIRECTION('ref_axis',(1.,0.,0.));
#11107=DIRECTION('',(0.,-1.,0.));
#11108=DIRECTION('',(1.,0.,0.));
#11109=DIRECTION('',(1.,0.,0.));
#11110=DIRECTION('',(0.,1.,0.));
#11111=DIRECTION('',(-1.,0.,0.));
#11112=DIRECTION('',(-1.,0.,0.));
#11113=DIRECTION('center_axis',(0.,0.,1.));
#11114=DIRECTION('ref_axis',(1.,0.,0.));
#11115=DIRECTION('center_axis',(0.,0.,1.));
#11116=DIRECTION('ref_axis',(1.,0.,0.));
#11117=DIRECTION('',(0.,0.,1.));
#11118=DIRECTION('center_axis',(0.,0.,1.));
#11119=DIRECTION('ref_axis',(1.,0.,0.));
#11120=DIRECTION('center_axis',(0.,0.,1.));
#11121=DIRECTION('ref_axis',(1.,0.,0.));
#11122=DIRECTION('',(0.,0.,1.));
#11123=DIRECTION('center_axis',(1.,0.,0.));
#11124=DIRECTION('ref_axis',(0.,0.,-1.));
#11125=DIRECTION('center_axis',(1.,0.,0.));
#11126=DIRECTION('ref_axis',(0.,0.,-1.));
#11127=DIRECTION('',(1.,0.,0.));
#11128=DIRECTION('',(1.,0.,0.));
#11129=DIRECTION('center_axis',(-1.,0.,0.));
#11130=DIRECTION('ref_axis',(0.,0.,-1.));
#11131=DIRECTION('center_axis',(0.,1.,0.));
#11132=DIRECTION('ref_axis',(-1.,0.,0.));
#11133=DIRECTION('',(-1.,0.,0.));
#11134=DIRECTION('',(0.,0.,1.));
#11135=DIRECTION('',(0.,0.,1.));
#11136=DIRECTION('center_axis',(1.,0.,0.));
#11137=DIRECTION('ref_axis',(0.,1.,0.));
#11138=DIRECTION('',(0.,1.,0.));
#11139=DIRECTION('',(0.,0.,1.));
#11140=DIRECTION('center_axis',(0.,-1.,0.));
#11141=DIRECTION('ref_axis',(1.,0.,0.));
#11142=DIRECTION('',(1.,0.,0.));
#11143=DIRECTION('',(0.,0.,1.));
#11144=DIRECTION('center_axis',(-1.,0.,0.));
#11145=DIRECTION('ref_axis',(0.,-1.,0.));
#11146=DIRECTION('',(0.,-1.,0.));
#11147=DIRECTION('center_axis',(0.,0.,1.));
#11148=DIRECTION('ref_axis',(1.,0.,0.));
#11149=DIRECTION('axis',(0.,0.,1.));
#11150=DIRECTION('refdir',(1.,0.,0.));
#11151=DIRECTION('center_axis',(0.,0.,1.));
#11152=DIRECTION('ref_axis',(1.,0.,0.));
#11153=DIRECTION('',(0.,0.,1.));
#11154=DIRECTION('center_axis',(0.,0.,1.));
#11155=DIRECTION('ref_axis',(1.,0.,0.));
#11156=DIRECTION('',(0.,0.,1.));
#11157=DIRECTION('center_axis',(0.,0.,-1.));
#11158=DIRECTION('ref_axis',(1.,0.,0.));
#11159=DIRECTION('center_axis',(0.,0.,1.));
#11160=DIRECTION('ref_axis',(1.,0.,0.));
#11161=DIRECTION('',(0.,0.,1.));
#11162=DIRECTION('center_axis',(0.,0.,1.));
#11163=DIRECTION('ref_axis',(1.,0.,0.));
#11164=DIRECTION('',(0.,0.,1.));
#11165=DIRECTION('center_axis',(0.,0.,-1.));
#11166=DIRECTION('ref_axis',(1.,0.,0.));
#11167=DIRECTION('center_axis',(0.,0.,1.));
#11168=DIRECTION('ref_axis',(1.,0.,0.));
#11169=DIRECTION('',(1.,0.,0.));
#11170=DIRECTION('center_axis',(0.,0.,1.));
#11171=DIRECTION('ref_axis',(1.,0.,0.));
#11172=DIRECTION('center_axis',(0.,0.,1.));
#11173=DIRECTION('ref_axis',(1.,0.,0.));
#11174=DIRECTION('center_axis',(0.,0.,1.));
#11175=DIRECTION('ref_axis',(1.,0.,0.));
#11176=DIRECTION('',(0.,0.,1.));
#11177=DIRECTION('center_axis',(0.,0.,-1.));
#11178=DIRECTION('ref_axis',(1.,0.,0.));
#11179=DIRECTION('center_axis',(0.,0.,1.));
#11180=DIRECTION('ref_axis',(1.,0.,0.));
#11181=DIRECTION('',(-1.,0.,0.));
#11182=DIRECTION('center_axis',(0.,0.,1.));
#11183=DIRECTION('ref_axis',(1.,0.,0.));
#11184=DIRECTION('center_axis',(0.,0.,-1.));
#11185=DIRECTION('ref_axis',(1.,0.,0.));
#11186=DIRECTION('',(0.,0.,1.));
#11187=DIRECTION('center_axis',(0.,0.,1.));
#11188=DIRECTION('ref_axis',(1.,0.,0.));
#11189=DIRECTION('center_axis',(0.,0.,1.));
#11190=DIRECTION('ref_axis',(1.,0.,0.));
#11191=DIRECTION('center_axis',(0.,0.,1.));
#11192=DIRECTION('ref_axis',(1.,0.,0.));
#11193=DIRECTION('center_axis',(0.,0.,1.));
#11194=DIRECTION('ref_axis',(1.,0.,0.));
#11195=DIRECTION('center_axis',(0.,0.,-1.));
#11196=DIRECTION('ref_axis',(1.,0.,0.));
#11197=DIRECTION('',(0.,0.,1.));
#11198=DIRECTION('center_axis',(0.,0.,1.));
#11199=DIRECTION('ref_axis',(1.,0.,0.));
#11200=DIRECTION('center_axis',(0.,0.,1.));
#11201=DIRECTION('ref_axis',(1.,0.,0.));
#11202=DIRECTION('center_axis',(0.,0.,1.));
#11203=DIRECTION('ref_axis',(1.,0.,0.));
#11204=DIRECTION('center_axis',(0.,0.,1.));
#11205=DIRECTION('ref_axis',(1.,0.,0.));
#11206=DIRECTION('',(0.,-1.,0.));
#11207=DIRECTION('',(1.,0.,0.));
#11208=DIRECTION('',(1.,0.,0.));
#11209=DIRECTION('',(0.,1.,0.));
#11210=DIRECTION('',(-1.,0.,0.));
#11211=DIRECTION('',(-1.,0.,0.));
#11212=DIRECTION('center_axis',(0.,0.,1.));
#11213=DIRECTION('ref_axis',(1.,0.,0.));
#11214=DIRECTION('center_axis',(0.,0.,1.));
#11215=DIRECTION('ref_axis',(1.,0.,0.));
#11216=DIRECTION('',(0.,0.,1.));
#11217=DIRECTION('center_axis',(0.,0.,1.));
#11218=DIRECTION('ref_axis',(1.,0.,0.));
#11219=DIRECTION('center_axis',(0.,0.,1.));
#11220=DIRECTION('ref_axis',(1.,0.,0.));
#11221=DIRECTION('',(0.,0.,1.));
#11222=DIRECTION('center_axis',(1.,0.,0.));
#11223=DIRECTION('ref_axis',(0.,0.,-1.));
#11224=DIRECTION('center_axis',(1.,0.,0.));
#11225=DIRECTION('ref_axis',(0.,0.,-1.));
#11226=DIRECTION('',(1.,0.,0.));
#11227=DIRECTION('',(1.,0.,0.));
#11228=DIRECTION('center_axis',(-1.,0.,0.));
#11229=DIRECTION('ref_axis',(0.,0.,-1.));
#11230=DIRECTION('center_axis',(0.,1.,0.));
#11231=DIRECTION('ref_axis',(-1.,0.,0.));
#11232=DIRECTION('',(-1.,0.,0.));
#11233=DIRECTION('',(0.,0.,1.));
#11234=DIRECTION('',(0.,0.,1.));
#11235=DIRECTION('center_axis',(1.,0.,0.));
#11236=DIRECTION('ref_axis',(0.,1.,0.));
#11237=DIRECTION('',(0.,1.,0.));
#11238=DIRECTION('',(0.,0.,1.));
#11239=DIRECTION('center_axis',(0.,-1.,0.));
#11240=DIRECTION('ref_axis',(1.,0.,0.));
#11241=DIRECTION('',(1.,0.,0.));
#11242=DIRECTION('',(0.,0.,1.));
#11243=DIRECTION('center_axis',(-1.,0.,0.));
#11244=DIRECTION('ref_axis',(0.,-1.,0.));
#11245=DIRECTION('',(0.,-1.,0.));
#11246=DIRECTION('center_axis',(0.,0.,1.));
#11247=DIRECTION('ref_axis',(1.,0.,0.));
#11248=DIRECTION('axis',(0.,0.,1.));
#11249=DIRECTION('refdir',(1.,0.,0.));
#11250=DIRECTION('center_axis',(0.,0.,1.));
#11251=DIRECTION('ref_axis',(1.,0.,0.));
#11252=DIRECTION('',(0.,0.,1.));
#11253=DIRECTION('center_axis',(0.,0.,1.));
#11254=DIRECTION('ref_axis',(1.,0.,0.));
#11255=DIRECTION('',(0.,0.,1.));
#11256=DIRECTION('center_axis',(0.,0.,-1.));
#11257=DIRECTION('ref_axis',(1.,0.,0.));
#11258=DIRECTION('center_axis',(0.,0.,1.));
#11259=DIRECTION('ref_axis',(1.,0.,0.));
#11260=DIRECTION('',(0.,1.,0.));
#11261=DIRECTION('center_axis',(0.,0.,1.));
#11262=DIRECTION('ref_axis',(1.,0.,0.));
#11263=DIRECTION('center_axis',(0.,0.,1.));
#11264=DIRECTION('ref_axis',(1.,0.,0.));
#11265=DIRECTION('center_axis',(0.,0.,1.));
#11266=DIRECTION('ref_axis',(1.,0.,0.));
#11267=DIRECTION('',(0.,0.,1.));
#11268=DIRECTION('center_axis',(0.,0.,-1.));
#11269=DIRECTION('ref_axis',(1.,0.,0.));
#11270=DIRECTION('center_axis',(0.,0.,1.));
#11271=DIRECTION('ref_axis',(1.,0.,0.));
#11272=DIRECTION('center_axis',(0.,0.,1.));
#11273=DIRECTION('ref_axis',(1.,0.,0.));
#11274=DIRECTION('',(0.,-1.,0.));
#11275=DIRECTION('center_axis',(0.,0.,1.));
#11276=DIRECTION('ref_axis',(1.,0.,0.));
#11277=DIRECTION('center_axis',(0.,0.,1.));
#11278=DIRECTION('ref_axis',(1.,0.,0.));
#11279=DIRECTION('',(0.,0.,1.));
#11280=DIRECTION('center_axis',(0.,0.,-1.));
#11281=DIRECTION('ref_axis',(1.,0.,0.));
#11282=DIRECTION('',(0.,0.,1.));
#11283=DIRECTION('center_axis',(0.,0.,1.));
#11284=DIRECTION('ref_axis',(1.,0.,0.));
#11285=DIRECTION('center_axis',(0.,0.,1.));
#11286=DIRECTION('ref_axis',(1.,0.,0.));
#11287=DIRECTION('center_axis',(0.,0.,1.));
#11288=DIRECTION('ref_axis',(1.,0.,0.));
#11289=DIRECTION('center_axis',(0.,0.,-1.));
#11290=DIRECTION('ref_axis',(1.,0.,0.));
#11291=DIRECTION('',(0.,0.,1.));
#11292=DIRECTION('center_axis',(0.,0.,1.));
#11293=DIRECTION('ref_axis',(1.,0.,0.));
#11294=DIRECTION('center_axis',(0.,0.,1.));
#11295=DIRECTION('ref_axis',(1.,0.,0.));
#11296=DIRECTION('center_axis',(0.,0.,1.));
#11297=DIRECTION('ref_axis',(1.,0.,0.));
#11298=DIRECTION('center_axis',(0.,0.,1.));
#11299=DIRECTION('ref_axis',(1.,0.,0.));
#11300=DIRECTION('',(0.,-1.,0.));
#11301=DIRECTION('',(0.,-1.,0.));
#11302=DIRECTION('',(1.,0.,0.));
#11303=DIRECTION('',(0.,1.,0.));
#11304=DIRECTION('',(0.,1.,0.));
#11305=DIRECTION('',(-1.,0.,0.));
#11306=DIRECTION('center_axis',(0.,0.,1.));
#11307=DIRECTION('ref_axis',(1.,0.,0.));
#11308=DIRECTION('center_axis',(0.,0.,1.));
#11309=DIRECTION('ref_axis',(1.,0.,0.));
#11310=DIRECTION('',(0.,0.,1.));
#11311=DIRECTION('center_axis',(0.,0.,1.));
#11312=DIRECTION('ref_axis',(1.,0.,0.));
#11313=DIRECTION('center_axis',(0.,0.,1.));
#11314=DIRECTION('ref_axis',(1.,0.,0.));
#11315=DIRECTION('',(0.,0.,1.));
#11316=DIRECTION('center_axis',(0.,1.,0.));
#11317=DIRECTION('ref_axis',(1.,0.,0.));
#11318=DIRECTION('center_axis',(0.,1.,0.));
#11319=DIRECTION('ref_axis',(1.,0.,0.));
#11320=DIRECTION('',(0.,1.,0.));
#11321=DIRECTION('center_axis',(0.,-1.,0.));
#11322=DIRECTION('ref_axis',(1.,0.,0.));
#11323=DIRECTION('center_axis',(0.,1.,0.));
#11324=DIRECTION('ref_axis',(-1.,0.,0.));
#11325=DIRECTION('',(-1.,0.,0.));
#11326=DIRECTION('',(0.,0.,1.));
#11327=DIRECTION('',(0.,0.,1.));
#11328=DIRECTION('center_axis',(1.,0.,0.));
#11329=DIRECTION('ref_axis',(0.,1.,0.));
#11330=DIRECTION('',(0.,1.,0.));
#11331=DIRECTION('',(0.,0.,1.));
#11332=DIRECTION('center_axis',(0.,-1.,0.));
#11333=DIRECTION('ref_axis',(1.,0.,0.));
#11334=DIRECTION('',(1.,0.,0.));
#11335=DIRECTION('',(0.,0.,1.));
#11336=DIRECTION('center_axis',(-1.,0.,0.));
#11337=DIRECTION('ref_axis',(0.,-1.,0.));
#11338=DIRECTION('',(0.,-1.,0.));
#11339=DIRECTION('center_axis',(0.,0.,1.));
#11340=DIRECTION('ref_axis',(1.,0.,0.));
#11341=DIRECTION('axis',(0.,0.,1.));
#11342=DIRECTION('refdir',(1.,0.,0.));
#11343=DIRECTION('center_axis',(0.,0.,1.));
#11344=DIRECTION('ref_axis',(1.,0.,0.));
#11345=DIRECTION('',(0.,0.,1.));
#11346=DIRECTION('center_axis',(0.,0.,1.));
#11347=DIRECTION('ref_axis',(1.,0.,0.));
#11348=DIRECTION('',(0.,0.,1.));
#11349=DIRECTION('center_axis',(0.,0.,-1.));
#11350=DIRECTION('ref_axis',(1.,0.,0.));
#11351=DIRECTION('center_axis',(0.,0.,1.));
#11352=DIRECTION('ref_axis',(1.,0.,0.));
#11353=DIRECTION('',(0.,1.,0.));
#11354=DIRECTION('center_axis',(0.,0.,1.));
#11355=DIRECTION('ref_axis',(1.,0.,0.));
#11356=DIRECTION('center_axis',(0.,0.,1.));
#11357=DIRECTION('ref_axis',(1.,0.,0.));
#11358=DIRECTION('center_axis',(0.,0.,1.));
#11359=DIRECTION('ref_axis',(1.,0.,0.));
#11360=DIRECTION('',(0.,0.,1.));
#11361=DIRECTION('center_axis',(0.,0.,-1.));
#11362=DIRECTION('ref_axis',(1.,0.,0.));
#11363=DIRECTION('center_axis',(0.,0.,1.));
#11364=DIRECTION('ref_axis',(1.,0.,0.));
#11365=DIRECTION('center_axis',(0.,0.,1.));
#11366=DIRECTION('ref_axis',(1.,0.,0.));
#11367=DIRECTION('',(0.,-1.,0.));
#11368=DIRECTION('center_axis',(0.,0.,1.));
#11369=DIRECTION('ref_axis',(1.,0.,0.));
#11370=DIRECTION('center_axis',(0.,0.,1.));
#11371=DIRECTION('ref_axis',(1.,0.,0.));
#11372=DIRECTION('',(0.,0.,1.));
#11373=DIRECTION('center_axis',(0.,0.,-1.));
#11374=DIRECTION('ref_axis',(1.,0.,0.));
#11375=DIRECTION('',(0.,0.,1.));
#11376=DIRECTION('center_axis',(0.,0.,1.));
#11377=DIRECTION('ref_axis',(1.,0.,0.));
#11378=DIRECTION('center_axis',(0.,0.,1.));
#11379=DIRECTION('ref_axis',(1.,0.,0.));
#11380=DIRECTION('center_axis',(0.,0.,1.));
#11381=DIRECTION('ref_axis',(1.,0.,0.));
#11382=DIRECTION('center_axis',(0.,0.,-1.));
#11383=DIRECTION('ref_axis',(1.,0.,0.));
#11384=DIRECTION('',(0.,0.,1.));
#11385=DIRECTION('center_axis',(0.,0.,1.));
#11386=DIRECTION('ref_axis',(1.,0.,0.));
#11387=DIRECTION('center_axis',(0.,0.,1.));
#11388=DIRECTION('ref_axis',(1.,0.,0.));
#11389=DIRECTION('center_axis',(0.,0.,1.));
#11390=DIRECTION('ref_axis',(1.,0.,0.));
#11391=DIRECTION('center_axis',(0.,0.,1.));
#11392=DIRECTION('ref_axis',(1.,0.,0.));
#11393=DIRECTION('',(0.,-1.,0.));
#11394=DIRECTION('',(0.,-1.,0.));
#11395=DIRECTION('',(1.,0.,0.));
#11396=DIRECTION('',(0.,1.,0.));
#11397=DIRECTION('',(0.,1.,0.));
#11398=DIRECTION('',(-1.,0.,0.));
#11399=DIRECTION('center_axis',(0.,0.,1.));
#11400=DIRECTION('ref_axis',(1.,0.,0.));
#11401=DIRECTION('center_axis',(0.,0.,1.));
#11402=DIRECTION('ref_axis',(1.,0.,0.));
#11403=DIRECTION('',(0.,0.,1.));
#11404=DIRECTION('center_axis',(0.,0.,1.));
#11405=DIRECTION('ref_axis',(1.,0.,0.));
#11406=DIRECTION('center_axis',(0.,0.,1.));
#11407=DIRECTION('ref_axis',(1.,0.,0.));
#11408=DIRECTION('',(0.,0.,1.));
#11409=DIRECTION('center_axis',(0.,1.,0.));
#11410=DIRECTION('ref_axis',(1.,0.,0.));
#11411=DIRECTION('center_axis',(0.,1.,0.));
#11412=DIRECTION('ref_axis',(1.,0.,0.));
#11413=DIRECTION('',(0.,1.,0.));
#11414=DIRECTION('center_axis',(0.,-1.,0.));
#11415=DIRECTION('ref_axis',(1.,0.,0.));
#11416=DIRECTION('center_axis',(0.,1.,0.));
#11417=DIRECTION('ref_axis',(-1.,0.,0.));
#11418=DIRECTION('',(-1.,0.,0.));
#11419=DIRECTION('',(0.,0.,1.));
#11420=DIRECTION('',(0.,0.,1.));
#11421=DIRECTION('center_axis',(1.,0.,0.));
#11422=DIRECTION('ref_axis',(0.,1.,0.));
#11423=DIRECTION('',(0.,1.,0.));
#11424=DIRECTION('',(0.,0.,1.));
#11425=DIRECTION('center_axis',(0.,-1.,0.));
#11426=DIRECTION('ref_axis',(1.,0.,0.));
#11427=DIRECTION('',(1.,0.,0.));
#11428=DIRECTION('',(0.,0.,1.));
#11429=DIRECTION('center_axis',(-1.,0.,0.));
#11430=DIRECTION('ref_axis',(0.,-1.,0.));
#11431=DIRECTION('',(0.,-1.,0.));
#11432=DIRECTION('center_axis',(0.,0.,1.));
#11433=DIRECTION('ref_axis',(1.,0.,0.));
#11434=DIRECTION('axis',(0.,0.,1.));
#11435=DIRECTION('refdir',(1.,0.,0.));
#11436=DIRECTION('center_axis',(0.866025403784439,0.,-0.5));
#11437=DIRECTION('ref_axis',(0.5,0.,0.866025403784439));
#11438=DIRECTION('',(-0.5,0.,-0.866025403784439));
#11439=DIRECTION('',(0.,-1.,0.));
#11440=DIRECTION('',(0.5,0.,0.866025403784439));
#11441=DIRECTION('',(0.,-1.,0.));
#11442=DIRECTION('center_axis',(1.20185167898973E-16,0.,-1.));
#11443=DIRECTION('ref_axis',(1.,0.,1.20185167898973E-16));
#11444=DIRECTION('',(-1.,0.,-1.20185167898973E-16));
#11445=DIRECTION('',(0.,-1.,0.));
#11446=DIRECTION('',(1.,0.,1.20185167898973E-16));
#11447=DIRECTION('center_axis',(-0.866025403784439,0.,-0.5));
#11448=DIRECTION('ref_axis',(0.5,0.,-0.866025403784439));
#11449=DIRECTION('',(-0.5,0.,0.866025403784439));
#11450=DIRECTION('',(0.,-1.,0.));
#11451=DIRECTION('',(0.5,0.,-0.866025403784439));
#11452=DIRECTION('center_axis',(-0.866025403784439,0.,0.5));
#11453=DIRECTION('ref_axis',(-0.5,0.,-0.866025403784439));
#11454=DIRECTION('',(0.5,0.,0.866025403784439));
#11455=DIRECTION('',(0.,-1.,0.));
#11456=DIRECTION('',(-0.5,0.,-0.866025403784439));
#11457=DIRECTION('center_axis',(-2.40370335797945E-16,0.,1.));
#11458=DIRECTION('ref_axis',(-1.,0.,-2.40370335797945E-16));
#11459=DIRECTION('',(1.,0.,2.40370335797945E-16));
#11460=DIRECTION('',(0.,-1.,0.));
#11461=DIRECTION('',(-1.,0.,-2.40370335797945E-16));
#11462=DIRECTION('center_axis',(0.866025403784439,0.,0.5));
#11463=DIRECTION('ref_axis',(-0.5,0.,0.866025403784439));
#11464=DIRECTION('',(0.5,0.,-0.866025403784439));
#11465=DIRECTION('',(-0.5,0.,0.866025403784439));
#11466=DIRECTION('center_axis',(0.,1.,0.));
#11467=DIRECTION('ref_axis',(1.,0.,0.));
#11468=DIRECTION('center_axis',(0.,-1.,0.));
#11469=DIRECTION('ref_axis',(0.,0.,-1.));
#11470=DIRECTION('center_axis',(0.,1.,0.));
#11471=DIRECTION('ref_axis',(1.,0.,0.));
#11472=DIRECTION('center_axis',(0.,1.,0.));
#11473=DIRECTION('ref_axis',(1.,0.,0.));
#11474=DIRECTION('center_axis',(0.,1.,0.));
#11475=DIRECTION('ref_axis',(0.,0.,1.));
#11476=DIRECTION('center_axis',(0.,-1.,0.));
#11477=DIRECTION('ref_axis',(1.,0.,0.));
#11478=DIRECTION('center_axis',(0.,-1.,0.));
#11479=DIRECTION('ref_axis',(1.,0.,0.));
#11480=DIRECTION('center_axis',(0.,-1.,0.));
#11481=DIRECTION('ref_axis',(1.,0.,0.));
#11482=DIRECTION('',(0.707106781186548,0.707106781186547,8.65956056235493E-17));
#11483=DIRECTION('center_axis',(0.,-1.,0.));
#11484=DIRECTION('ref_axis',(1.,0.,0.));
#11485=DIRECTION('center_axis',(0.,-1.,0.));
#11486=DIRECTION('ref_axis',(1.,0.,0.));
#11487=DIRECTION('',(0.,1.,0.));
#11488=DIRECTION('center_axis',(0.,1.,0.));
#11489=DIRECTION('ref_axis',(1.,0.,0.));
#11490=DIRECTION('center_axis',(0.,-1.,0.));
#11491=DIRECTION('ref_axis',(1.,0.,0.));
#11492=DIRECTION('',(-0.707106781186547,0.707106781186548,-8.65956056235493E-17));
#11493=DIRECTION('center_axis',(0.,-1.,0.));
#11494=DIRECTION('ref_axis',(0.,0.,-1.));
#11495=DIRECTION('center_axis',(0.,-1.,0.));
#11496=DIRECTION('ref_axis',(1.,0.,0.));
#11497=DIRECTION('center_axis',(0.,1.,0.));
#11498=DIRECTION('ref_axis',(1.,0.,0.));
#11499=DIRECTION('center_axis',(0.,1.,0.));
#11500=DIRECTION('ref_axis',(1.,0.,0.));
#11501=DIRECTION('',(-0.447213595499958,0.894427190999916,-5.47678698264203E-17));
#11502=DIRECTION('center_axis',(0.,-1.,0.));
#11503=DIRECTION('ref_axis',(1.,0.,0.));
#11504=DIRECTION('',(0.,1.,0.));
#11505=DIRECTION('axis',(0.,0.,1.));
#11506=DIRECTION('refdir',(1.,0.,0.));
#11507=DIRECTION('axis',(0.,0.,1.));
#11508=DIRECTION('refdir',(1.,0.,0.));
#11509=DIRECTION('center_axis',(0.,-1.,0.));
#11510=DIRECTION('ref_axis',(0.,0.,-1.));
#11511=DIRECTION('center_axis',(0.,-1.,0.));
#11512=DIRECTION('ref_axis',(1.,0.,0.));
#11513=DIRECTION('center_axis',(0.,-1.,0.));
#11514=DIRECTION('ref_axis',(1.,0.,0.));
#11515=DIRECTION('center_axis',(1.,0.,1.22464679914735E-16));
#11516=DIRECTION('ref_axis',(-1.22464679914735E-16,0.,1.));
#11517=DIRECTION('center_axis',(0.,1.,0.));
#11518=DIRECTION('ref_axis',(1.,0.,0.));
#11519=DIRECTION('center_axis',(0.,1.,0.));
#11520=DIRECTION('ref_axis',(1.,0.,0.));
#11521=DIRECTION('center_axis',(0.,-1.,0.));
#11522=DIRECTION('ref_axis',(1.,0.,0.));
#11523=DIRECTION('',(0.,1.,0.));
#11524=DIRECTION('center_axis',(0.,-1.,0.));
#11525=DIRECTION('ref_axis',(1.,0.,0.));
#11526=DIRECTION('center_axis',(0.,-1.,0.));
#11527=DIRECTION('ref_axis',(1.,0.,0.));
#11528=DIRECTION('center_axis',(0.,-1.,0.));
#11529=DIRECTION('ref_axis',(1.,0.,0.));
#11530=DIRECTION('',(0.,1.,0.));
#11531=DIRECTION('center_axis',(0.,-1.,0.));
#11532=DIRECTION('ref_axis',(1.,0.,0.));
#11533=DIRECTION('center_axis',(0.,1.,0.));
#11534=DIRECTION('ref_axis',(1.,0.,0.));
#11535=DIRECTION('',(-0.707106781186547,0.707106781186548,-8.65956056235493E-17));
#11536=DIRECTION('center_axis',(0.,-1.,0.));
#11537=DIRECTION('ref_axis',(1.,0.,0.));
#11538=DIRECTION('center_axis',(0.,1.,0.));
#11539=DIRECTION('ref_axis',(0.,0.,1.));
#11540=DIRECTION('center_axis',(0.,-1.,0.));
#11541=DIRECTION('ref_axis',(1.,0.,0.));
#11542=DIRECTION('center_axis',(0.,-1.,0.));
#11543=DIRECTION('ref_axis',(1.,0.,0.));
#11544=DIRECTION('',(0.,1.,0.));
#11545=DIRECTION('center_axis',(0.,-1.,0.));
#11546=DIRECTION('ref_axis',(0.,0.,-1.));
#11547=DIRECTION('center_axis',(0.,-1.,0.));
#11548=DIRECTION('ref_axis',(1.,0.,0.));
#11549=DIRECTION('center_axis',(0.,-1.,0.));
#11550=DIRECTION('ref_axis',(1.,0.,0.));
#11551=DIRECTION('',(0.707106781186547,0.707106781186548,8.65956056235493E-17));
#11552=DIRECTION('axis',(0.,0.,1.));
#11553=DIRECTION('refdir',(1.,0.,0.));
#11554=DIRECTION('center_axis',(0.,-1.,0.));
#11555=DIRECTION('ref_axis',(0.,0.,-1.));
#11556=DIRECTION('center_axis',(0.,-1.,0.));
#11557=DIRECTION('ref_axis',(1.,0.,0.));
#11558=DIRECTION('center_axis',(0.,-1.,0.));
#11559=DIRECTION('ref_axis',(1.,0.,0.));
#11560=DIRECTION('center_axis',(1.,0.,1.22464679914735E-16));
#11561=DIRECTION('ref_axis',(-1.22464679914735E-16,0.,1.));
#11562=DIRECTION('center_axis',(0.,1.,0.));
#11563=DIRECTION('ref_axis',(1.,0.,0.));
#11564=DIRECTION('center_axis',(0.,1.,0.));
#11565=DIRECTION('ref_axis',(1.,0.,0.));
#11566=DIRECTION('center_axis',(0.,-1.,0.));
#11567=DIRECTION('ref_axis',(1.,0.,0.));
#11568=DIRECTION('center_axis',(0.,-1.,0.));
#11569=DIRECTION('ref_axis',(1.,0.,0.));
#11570=DIRECTION('',(0.,1.,0.));
#11571=DIRECTION('center_axis',(0.,1.,0.));
#11572=DIRECTION('ref_axis',(0.,0.,1.));
#11573=DIRECTION('center_axis',(0.,-1.,0.));
#11574=DIRECTION('ref_axis',(1.,0.,0.));
#11575=DIRECTION('center_axis',(0.,-1.,0.));
#11576=DIRECTION('ref_axis',(1.,0.,0.));
#11577=DIRECTION('center_axis',(0.,-1.,0.));
#11578=DIRECTION('ref_axis',(1.,0.,0.));
#11579=DIRECTION('center_axis',(0.,-1.,0.));
#11580=DIRECTION('ref_axis',(1.,0.,0.));
#11581=DIRECTION('',(0.707106781186548,0.707106781186547,8.65956056235494E-17));
#11582=DIRECTION('center_axis',(0.,-1.,0.));
#11583=DIRECTION('ref_axis',(1.,0.,0.));
#11584=DIRECTION('center_axis',(0.,-1.,0.));
#11585=DIRECTION('ref_axis',(1.,0.,0.));
#11586=DIRECTION('',(0.,1.,0.));
#11587=DIRECTION('center_axis',(0.,1.,0.));
#11588=DIRECTION('ref_axis',(1.,0.,0.));
#11589=DIRECTION('center_axis',(0.,-1.,0.));
#11590=DIRECTION('ref_axis',(1.,0.,0.));
#11591=DIRECTION('',(-0.707106781186548,0.707106781186547,-8.65956056235494E-17));
#11592=DIRECTION('center_axis',(0.,-1.,0.));
#11593=DIRECTION('ref_axis',(0.,0.,-1.));
#11594=DIRECTION('center_axis',(0.,-1.,0.));
#11595=DIRECTION('ref_axis',(1.,0.,0.));
#11596=DIRECTION('',(0.,1.,0.));
#11597=DIRECTION('axis',(0.,0.,1.));
#11598=DIRECTION('refdir',(1.,0.,0.));
#11599=DIRECTION('center_axis',(0.,0.,1.));
#11600=DIRECTION('ref_axis',(1.,0.,0.));
#11601=DIRECTION('center_axis',(1.22464679914735E-16,-1.,0.));
#11602=DIRECTION('ref_axis',(-1.,-1.22464679914735E-16,0.));
#11603=DIRECTION('center_axis',(0.707106781186548,0.,0.707106781186548));
#11604=DIRECTION('ref_axis',(0.707106781186548,0.,-0.707106781186548));
#11605=DIRECTION('center_axis',(8.65956056235494E-17,-1.,-8.65956056235493E-17));
#11606=DIRECTION('ref_axis',(-0.707106781186547,-1.22464679914735E-16,0.707106781186547));
#11607=DIRECTION('center_axis',(1.,0.,0.));
#11608=DIRECTION('ref_axis',(6.12323399573676E-17,0.,-1.));
#11609=DIRECTION('center_axis',(7.49879891330929E-33,-1.,-1.22464679914735E-16));
#11610=DIRECTION('ref_axis',(-6.12323399573676E-17,-1.22464679914735E-16,
1.));
#11611=DIRECTION('center_axis',(0.707106781186548,0.,-0.707106781186548));
#11612=DIRECTION('ref_axis',(-0.707106781186548,0.,-0.707106781186548));
#11613=DIRECTION('center_axis',(-8.65956056235493E-17,-1.,-8.65956056235494E-17));
#11614=DIRECTION('ref_axis',(0.707106781186547,-1.22464679914735E-16,0.707106781186547));
#11615=DIRECTION('center_axis',(0.,0.,-1.));
#11616=DIRECTION('ref_axis',(-1.,0.,-1.22464679914735E-16));
#11617=DIRECTION('center_axis',(-1.22464679914735E-16,-1.,-1.49975978266186E-32));
#11618=DIRECTION('ref_axis',(1.,-1.22464679914735E-16,1.22464679914735E-16));
#11619=DIRECTION('center_axis',(-0.707106781186547,0.,-0.707106781186548));
#11620=DIRECTION('ref_axis',(-0.707106781186548,0.,0.707106781186547));
#11621=DIRECTION('center_axis',(-8.65956056235493E-17,-1.,8.65956056235493E-17));
#11622=DIRECTION('ref_axis',(0.707106781186548,-1.22464679914735E-16,-0.707106781186547));
#11623=DIRECTION('center_axis',(-1.,0.,0.));
#11624=DIRECTION('ref_axis',(-1.83697019872103E-16,0.,1.));
#11625=DIRECTION('center_axis',(-2.24963967399279E-32,-1.,1.22464679914735E-16));
#11626=DIRECTION('ref_axis',(1.83697019872103E-16,-1.22464679914735E-16,
-1.));
#11627=DIRECTION('center_axis',(-0.707106781186548,0.,0.707106781186548));
#11628=DIRECTION('ref_axis',(0.707106781186547,0.,0.707106781186548));
#11629=DIRECTION('center_axis',(8.65956056235493E-17,-1.,8.65956056235493E-17));
#11630=DIRECTION('ref_axis',(-0.707106781186547,-1.22464679914735E-16,-0.707106781186548));
#11631=DIRECTION('axis',(0.,0.,1.));
#11632=DIRECTION('refdir',(1.,0.,0.));
#11633=DIRECTION('center_axis',(0.,0.,1.));
#11634=DIRECTION('ref_axis',(1.,0.,0.));
#11635=DIRECTION('center_axis',(0.,-1.,0.));
#11636=DIRECTION('ref_axis',(0.,0.,-1.));
#11637=DIRECTION('center_axis',(0.,-1.,0.));
#11638=DIRECTION('ref_axis',(0.,0.,-1.));
#11639=DIRECTION('center_axis',(0.,1.,0.));
#11640=DIRECTION('ref_axis',(1.,0.,0.));
#11641=DIRECTION('center_axis',(0.,1.,0.));
#11642=DIRECTION('ref_axis',(1.,0.,0.));
#11643=DIRECTION('center_axis',(0.,1.,0.));
#11644=DIRECTION('ref_axis',(1.,0.,0.));
#11645=DIRECTION('center_axis',(0.,1.,0.));
#11646=DIRECTION('ref_axis',(1.,0.,0.));
#11647=DIRECTION('',(0.,-1.,0.));
#11648=DIRECTION('center_axis',(0.,-1.,0.));
#11649=DIRECTION('ref_axis',(1.,0.,0.));
#11650=DIRECTION('center_axis',(0.,1.,0.));
#11651=DIRECTION('ref_axis',(1.,0.,0.));
#11652=DIRECTION('center_axis',(0.,1.,0.));
#11653=DIRECTION('ref_axis',(1.,0.,0.));
#11654=DIRECTION('center_axis',(0.,1.,0.));
#11655=DIRECTION('ref_axis',(1.,0.,0.));
#11656=DIRECTION('center_axis',(0.,1.,0.));
#11657=DIRECTION('ref_axis',(1.,0.,0.));
#11658=DIRECTION('center_axis',(0.,1.,0.));
#11659=DIRECTION('ref_axis',(1.,0.,0.));
#11660=DIRECTION('center_axis',(0.,1.,0.));
#11661=DIRECTION('ref_axis',(1.,0.,0.));
#11662=DIRECTION('center_axis',(0.,-1.,0.));
#11663=DIRECTION('ref_axis',(1.,0.,0.));
#11664=DIRECTION('center_axis',(0.,-1.,0.));
#11665=DIRECTION('ref_axis',(0.,0.,-1.));
#11666=DIRECTION('center_axis',(6.12323399573677E-17,0.,1.));
#11667=DIRECTION('ref_axis',(1.,0.,0.));
#11668=DIRECTION('center_axis',(0.,-1.,0.));
#11669=DIRECTION('ref_axis',(0.,0.,-1.));
#11670=DIRECTION('center_axis',(0.,1.,0.));
#11671=DIRECTION('ref_axis',(1.,0.,0.));
#11672=DIRECTION('center_axis',(0.,-1.,0.));
#11673=DIRECTION('ref_axis',(1.,0.,0.));
#11674=DIRECTION('center_axis',(0.,-1.,0.));
#11675=DIRECTION('ref_axis',(0.,0.,-1.));
#11676=DIRECTION('center_axis',(0.,0.,1.));
#11677=DIRECTION('ref_axis',(1.,0.,0.));
#11678=DIRECTION('center_axis',(0.,-1.,0.));
#11679=DIRECTION('ref_axis',(0.,0.,-1.));
#11680=DIRECTION('center_axis',(0.,1.,0.));
#11681=DIRECTION('ref_axis',(1.,0.,0.));
#11682=DIRECTION('center_axis',(0.,-1.,0.));
#11683=DIRECTION('ref_axis',(1.,0.,0.));
#11684=DIRECTION('center_axis',(0.,-1.,0.));
#11685=DIRECTION('ref_axis',(0.,0.,-1.));
#11686=DIRECTION('center_axis',(0.,0.,1.));
#11687=DIRECTION('ref_axis',(1.,0.,0.));
#11688=DIRECTION('center_axis',(0.,-1.,0.));
#11689=DIRECTION('ref_axis',(0.,0.,-1.));
#11690=DIRECTION('center_axis',(0.,1.,0.));
#11691=DIRECTION('ref_axis',(1.,0.,0.));
#11692=DIRECTION('center_axis',(0.,-1.,0.));
#11693=DIRECTION('ref_axis',(1.,0.,0.));
#11694=DIRECTION('center_axis',(0.,-1.,0.));
#11695=DIRECTION('ref_axis',(0.,0.,-1.));
#11696=DIRECTION('center_axis',(0.,0.,1.));
#11697=DIRECTION('ref_axis',(1.,0.,0.));
#11698=DIRECTION('center_axis',(0.,-1.,0.));
#11699=DIRECTION('ref_axis',(0.,0.,-1.));
#11700=DIRECTION('center_axis',(0.,1.,0.));
#11701=DIRECTION('ref_axis',(1.,0.,0.));
#11702=DIRECTION('center_axis',(0.,-1.,0.));
#11703=DIRECTION('ref_axis',(1.,0.,0.));
#11704=DIRECTION('center_axis',(0.,-1.,0.));
#11705=DIRECTION('ref_axis',(0.,0.,-1.));
#11706=DIRECTION('center_axis',(6.12323399573676E-17,0.,1.));
#11707=DIRECTION('ref_axis',(1.,0.,0.));
#11708=DIRECTION('center_axis',(0.,-1.,0.));
#11709=DIRECTION('ref_axis',(0.,0.,-1.));
#11710=DIRECTION('center_axis',(0.,1.,0.));
#11711=DIRECTION('ref_axis',(1.,0.,0.));
#11712=DIRECTION('center_axis',(0.,-1.,0.));
#11713=DIRECTION('ref_axis',(1.,0.,0.));
#11714=DIRECTION('center_axis',(0.,-1.,0.));
#11715=DIRECTION('ref_axis',(0.,0.,-1.));
#11716=DIRECTION('center_axis',(0.,0.,1.));
#11717=DIRECTION('ref_axis',(1.,0.,0.));
#11718=DIRECTION('center_axis',(0.,-1.,0.));
#11719=DIRECTION('ref_axis',(0.,0.,-1.));
#11720=DIRECTION('center_axis',(0.,1.,0.));
#11721=DIRECTION('ref_axis',(1.,0.,0.));
#11722=DIRECTION('center_axis',(0.,1.,0.));
#11723=DIRECTION('ref_axis',(1.,0.,0.));
#11724=DIRECTION('',(0.,1.,0.));
#11725=DIRECTION('center_axis',(0.,-1.,0.));
#11726=DIRECTION('ref_axis',(1.,0.,0.));
#11727=DIRECTION('center_axis',(0.,-1.,0.));
#11728=DIRECTION('ref_axis',(1.,0.,0.));
#11729=DIRECTION('center_axis',(0.,1.,0.));
#11730=DIRECTION('ref_axis',(1.,0.,0.));
#11731=DIRECTION('center_axis',(0.,-1.,0.));
#11732=DIRECTION('ref_axis',(0.,0.,-1.));
#11733=DIRECTION('center_axis',(0.,0.,1.));
#11734=DIRECTION('ref_axis',(1.,0.,0.));
#11735=DIRECTION('center_axis',(0.,-1.,0.));
#11736=DIRECTION('ref_axis',(0.,0.,-1.));
#11737=DIRECTION('center_axis',(0.,-1.,0.));
#11738=DIRECTION('ref_axis',(-1.,0.,0.));
#11739=DIRECTION('center_axis',(0.,1.,0.));
#11740=DIRECTION('ref_axis',(1.,0.,0.));
#11741=DIRECTION('axis',(0.,0.,1.));
#11742=DIRECTION('refdir',(1.,0.,0.));
#11743=DIRECTION('center_axis',(0.,1.,0.));
#11744=DIRECTION('ref_axis',(0.,0.,1.));
#11745=DIRECTION('center_axis',(0.,-1.,0.));
#11746=DIRECTION('ref_axis',(1.,0.,0.));
#11747=DIRECTION('center_axis',(0.,-1.,0.));
#11748=DIRECTION('ref_axis',(1.,0.,0.));
#11749=DIRECTION('center_axis',(0.,-1.,0.));
#11750=DIRECTION('ref_axis',(1.,0.,0.));
#11751=DIRECTION('center_axis',(0.,-1.,0.));
#11752=DIRECTION('ref_axis',(1.,0.,0.));
#11753=DIRECTION('',(0.,1.,0.));
#11754=DIRECTION('center_axis',(0.,-1.,0.));
#11755=DIRECTION('ref_axis',(0.,0.,-1.));
#11756=DIRECTION('center_axis',(0.,-1.,0.));
#11757=DIRECTION('ref_axis',(1.,0.,0.));
#11758=DIRECTION('center_axis',(0.,-1.,0.));
#11759=DIRECTION('ref_axis',(1.,0.,0.));
#11760=DIRECTION('',(0.,1.,0.));
#11761=DIRECTION('center_axis',(0.,1.,0.));
#11762=DIRECTION('ref_axis',(0.,0.,1.));
#11763=DIRECTION('center_axis',(0.,-1.,0.));
#11764=DIRECTION('ref_axis',(1.,0.,0.));
#11765=DIRECTION('center_axis',(0.,-1.,0.));
#11766=DIRECTION('ref_axis',(1.,0.,0.));
#11767=DIRECTION('center_axis',(0.,-1.,0.));
#11768=DIRECTION('ref_axis',(1.,0.,0.));
#11769=DIRECTION('center_axis',(0.,-1.,0.));
#11770=DIRECTION('ref_axis',(1.,0.,0.));
#11771=DIRECTION('',(0.,1.,0.));
#11772=DIRECTION('center_axis',(0.,-1.,0.));
#11773=DIRECTION('ref_axis',(0.,0.,-1.));
#11774=DIRECTION('center_axis',(0.,-1.,0.));
#11775=DIRECTION('ref_axis',(1.,0.,0.));
#11776=DIRECTION('center_axis',(0.,-1.,0.));
#11777=DIRECTION('ref_axis',(1.,0.,0.));
#11778=DIRECTION('',(0.,1.,0.));
#11779=DIRECTION('',(0.,0.,1.));
#11780=DIRECTION('',(1.,0.,0.));
#11781=DIRECTION('',(0.,0.,1.));
#11782=DIRECTION('',(1.,0.,0.));
#11783=DIRECTION('',(0.,0.,1.));
#11784=DIRECTION('',(1.,0.,0.));
#11785=DIRECTION('',(0.,0.,1.));
#11786=DIRECTION('',(1.,0.,0.));
#11787=DIRECTION('',(0.,0.,1.));
#11788=DIRECTION('',(1.,0.,0.));
#11789=DIRECTION('axis',(0.,0.,1.));
#11790=DIRECTION('refdir',(1.,0.,0.));
#11791=DIRECTION('center_axis',(1.,0.,0.));
#11792=DIRECTION('ref_axis',(0.,0.,-1.));
#11793=DIRECTION('center_axis',(-1.,0.,0.));
#11794=DIRECTION('ref_axis',(0.,0.,-1.));
#11795=DIRECTION('center_axis',(1.,0.,0.));
#11796=DIRECTION('ref_axis',(0.,0.,-1.));
#11797=DIRECTION('center_axis',(-1.,0.,0.));
#11798=DIRECTION('ref_axis',(0.,0.,-1.));
#11799=DIRECTION('',(-0.707106781186548,8.65956056235493E-17,-0.707106781186547));
#11800=DIRECTION('center_axis',(1.,0.,0.));
#11801=DIRECTION('ref_axis',(0.,0.,-1.));
#11802=DIRECTION('center_axis',(1.,0.,0.));
#11803=DIRECTION('ref_axis',(0.,0.,-1.));
#11804=DIRECTION('',(-1.,0.,0.));
#11805=DIRECTION('center_axis',(1.,0.,0.));
#11806=DIRECTION('ref_axis',(0.,0.,-1.));
#11807=DIRECTION('axis',(0.,0.,1.));
#11808=DIRECTION('refdir',(1.,0.,0.));
#11809=DIRECTION('center_axis',(0.866025403784439,0.,-0.5));
#11810=DIRECTION('ref_axis',(0.5,0.,0.866025403784439));
#11811=DIRECTION('',(0.5,0.,0.866025403784439));
#11812=DIRECTION('',(0.,-1.,0.));
#11813=DIRECTION('',(0.5,0.,0.866025403784439));
#11814=DIRECTION('',(0.,-1.,0.));
#11815=DIRECTION('center_axis',(1.20185167898973E-16,0.,-1.));
#11816=DIRECTION('ref_axis',(1.,0.,1.20185167898973E-16));
#11817=DIRECTION('',(1.,0.,1.20185167898973E-16));
#11818=DIRECTION('',(0.,-1.,0.));
#11819=DIRECTION('',(1.,0.,1.20185167898973E-16));
#11820=DIRECTION('center_axis',(-0.866025403784439,0.,-0.5));
#11821=DIRECTION('ref_axis',(0.5,0.,-0.866025403784439));
#11822=DIRECTION('',(0.5,0.,-0.866025403784439));
#11823=DIRECTION('',(0.,-1.,0.));
#11824=DIRECTION('',(0.5,0.,-0.866025403784439));
#11825=DIRECTION('center_axis',(-0.866025403784439,0.,0.5));
#11826=DIRECTION('ref_axis',(-0.5,0.,-0.866025403784439));
#11827=DIRECTION('',(-0.5,0.,-0.866025403784439));
#11828=DIRECTION('',(0.,-1.,0.));
#11829=DIRECTION('',(-0.5,0.,-0.866025403784439));
#11830=DIRECTION('center_axis',(-2.40370335797945E-16,0.,1.));
#11831=DIRECTION('ref_axis',(-1.,0.,-2.40370335797945E-16));
#11832=DIRECTION('',(-1.,0.,-2.40370335797945E-16));
#11833=DIRECTION('',(0.,-1.,0.));
#11834=DIRECTION('',(-1.,0.,-2.40370335797945E-16));
#11835=DIRECTION('center_axis',(0.866025403784439,0.,0.5));
#11836=DIRECTION('ref_axis',(-0.5,0.,0.866025403784439));
#11837=DIRECTION('',(-0.5,0.,0.866025403784439));
#11838=DIRECTION('',(-0.5,0.,0.866025403784439));
#11839=DIRECTION('center_axis',(0.,-1.,0.));
#11840=DIRECTION('ref_axis',(0.,0.,-1.));
#11841=DIRECTION('center_axis',(0.,1.,0.));
#11842=DIRECTION('ref_axis',(0.,0.,1.));
#11843=DIRECTION('center_axis',(0.,-1.,0.));
#11844=DIRECTION('ref_axis',(1.,0.,0.));
#11845=DIRECTION('center_axis',(0.,-1.,0.));
#11846=DIRECTION('ref_axis',(1.,0.,0.));
#11847=DIRECTION('center_axis',(0.,-1.,0.));
#11848=DIRECTION('ref_axis',(1.,0.,0.));
#11849=DIRECTION('',(0.707106781186548,0.707106781186547,8.65956056235494E-17));
#11850=DIRECTION('center_axis',(0.,-1.,0.));
#11851=DIRECTION('ref_axis',(1.,0.,0.));
#11852=DIRECTION('center_axis',(0.,1.,0.));
#11853=DIRECTION('ref_axis',(1.,0.,0.));
#11854=DIRECTION('',(0.,1.,0.));
#11855=DIRECTION('center_axis',(0.,1.,0.));
#11856=DIRECTION('ref_axis',(1.,0.,0.));
#11857=DIRECTION('center_axis',(0.,-1.,0.));
#11858=DIRECTION('ref_axis',(1.,0.,0.));
#11859=DIRECTION('',(-0.707106781186548,0.707106781186547,-8.65956056235494E-17));
#11860=DIRECTION('center_axis',(0.,-1.,0.));
#11861=DIRECTION('ref_axis',(0.,0.,-1.));
#11862=DIRECTION('axis',(0.,0.,1.));
#11863=DIRECTION('refdir',(1.,0.,0.));
#11864=DIRECTION('axis',(0.,0.,1.));
#11865=DIRECTION('refdir',(1.,0.,0.));
#11866=DIRECTION('center_axis',(0.,0.,1.));
#11867=DIRECTION('ref_axis',(1.,0.,0.));
#11868=DIRECTION('center_axis',(0.,0.,1.));
#11869=DIRECTION('ref_axis',(1.,0.,0.));
#11870=DIRECTION('',(0.,0.,1.));
#11871=DIRECTION('center_axis',(0.,0.,-1.));
#11872=DIRECTION('ref_axis',(1.,0.,0.));
#11873=DIRECTION('center_axis',(0.,0.,1.));
#11874=DIRECTION('ref_axis',(1.,0.,0.));
#11875=DIRECTION('center_axis',(0.,0.,1.));
#11876=DIRECTION('ref_axis',(1.,0.,0.));
#11877=DIRECTION('',(0.,0.,1.));
#11878=DIRECTION('center_axis',(0.,0.,-1.));
#11879=DIRECTION('ref_axis',(1.,0.,0.));
#11880=DIRECTION('center_axis',(0.,0.,1.));
#11881=DIRECTION('ref_axis',(1.,0.,0.));
#11882=DIRECTION('center_axis',(0.,0.,1.));
#11883=DIRECTION('ref_axis',(1.,0.,0.));
#11884=DIRECTION('',(0.,0.,1.));
#11885=DIRECTION('center_axis',(0.,0.,-1.));
#11886=DIRECTION('ref_axis',(1.,0.,0.));
#11887=DIRECTION('center_axis',(0.,0.,1.));
#11888=DIRECTION('ref_axis',(-0.707106781186548,-0.707106781186547,0.));
#11889=DIRECTION('',(0.,0.,1.));
#11890=DIRECTION('center_axis',(0.,0.,1.));
#11891=DIRECTION('ref_axis',(1.,0.,0.));
#11892=DIRECTION('',(0.,0.,-1.));
#11893=DIRECTION('center_axis',(0.,0.,1.));
#11894=DIRECTION('ref_axis',(1.,0.,0.));
#11895=DIRECTION('center_axis',(-0.707106781186548,0.707106781186548,0.));
#11896=DIRECTION('ref_axis',(-0.707106781186548,-0.707106781186548,0.));
#11897=DIRECTION('',(-0.707106781186548,-0.707106781186548,0.));
#11898=DIRECTION('',(0.,0.,1.));
#11899=DIRECTION('',(0.707106781186548,0.707106781186548,0.));
#11900=DIRECTION('center_axis',(0.,0.,1.));
#11901=DIRECTION('ref_axis',(1.,0.,0.));
#11902=DIRECTION('',(0.707106781186548,0.707106781186548,0.));
#11903=DIRECTION('center_axis',(0.,0.,1.));
#11904=DIRECTION('ref_axis',(1.,0.,0.));
#11905=DIRECTION('',(1.,0.,0.));
#11906=DIRECTION('center_axis',(0.,0.,1.));
#11907=DIRECTION('ref_axis',(1.,0.,0.));
#11908=DIRECTION('',(-1.,0.,0.));
#11909=DIRECTION('center_axis',(0.,0.,1.));
#11910=DIRECTION('ref_axis',(1.,0.,0.));
#11911=DIRECTION('',(0.,1.,0.));
#11912=DIRECTION('center_axis',(0.,0.,1.));
#11913=DIRECTION('ref_axis',(1.,0.,0.));
#11914=DIRECTION('',(0.,-1.,0.));
#11915=DIRECTION('center_axis',(0.,0.,1.));
#11916=DIRECTION('ref_axis',(1.,0.,0.));
#11917=DIRECTION('center_axis',(0.707106781186548,-0.707106781186548,0.));
#11918=DIRECTION('ref_axis',(0.707106781186548,0.707106781186548,0.));
#11919=DIRECTION('',(-0.707106781186548,-0.707106781186548,0.));
#11920=DIRECTION('',(0.,0.,-1.));
#11921=DIRECTION('center_axis',(0.,0.,1.));
#11922=DIRECTION('ref_axis',(-0.923879532511287,0.38268343236509,0.));
#11923=DIRECTION('',(0.,0.,-1.));
#11924=DIRECTION('center_axis',(0.,0.,1.));
#11925=DIRECTION('ref_axis',(1.,0.,0.));
#11926=DIRECTION('center_axis',(0.,0.,1.));
#11927=DIRECTION('ref_axis',(1.,0.,0.));
#11928=DIRECTION('center_axis',(0.,0.,1.));
#11929=DIRECTION('ref_axis',(1.,0.,0.));
#11930=DIRECTION('',(0.,0.,1.));
#11931=DIRECTION('center_axis',(0.,0.,1.));
#11932=DIRECTION('ref_axis',(1.,0.,0.));
#11933=DIRECTION('',(0.,0.,-1.));
#11934=DIRECTION('',(0.,0.,1.));
#11935=DIRECTION('center_axis',(0.,0.,1.));
#11936=DIRECTION('ref_axis',(1.,0.,0.));
#11937=DIRECTION('center_axis',(0.,1.,0.));
#11938=DIRECTION('ref_axis',(-1.,0.,0.));
#11939=DIRECTION('',(1.,0.,0.));
#11940=DIRECTION('',(0.,0.,-1.));
#11941=DIRECTION('center_axis',(0.,0.,1.));
#11942=DIRECTION('ref_axis',(1.,0.,0.));
#11943=DIRECTION('',(0.,1.,0.));
#11944=DIRECTION('center_axis',(0.,0.,1.));
#11945=DIRECTION('ref_axis',(1.,0.,0.));
#11946=DIRECTION('',(0.,-1.,0.));
#11947=DIRECTION('center_axis',(0.,0.,1.));
#11948=DIRECTION('ref_axis',(1.,0.,0.));
#11949=DIRECTION('',(-1.,0.,0.));
#11950=DIRECTION('center_axis',(0.,0.,1.));
#11951=DIRECTION('ref_axis',(1.,0.,0.));
#11952=DIRECTION('center_axis',(0.,-1.,0.));
#11953=DIRECTION('ref_axis',(1.,0.,0.));
#11954=DIRECTION('center_axis',(0.,0.,1.));
#11955=DIRECTION('ref_axis',(6.12323399573677E-17,1.,0.));
#11956=DIRECTION('',(0.,0.,1.));
#11957=DIRECTION('',(0.,0.,-1.));
#11958=DIRECTION('center_axis',(1.,0.,0.));
#11959=DIRECTION('ref_axis',(0.,1.,0.));
#11960=DIRECTION('',(0.,0.,1.));
#11961=DIRECTION('center_axis',(-1.,0.,0.));
#11962=DIRECTION('ref_axis',(0.,-1.,0.));
#11963=DIRECTION('center_axis',(0.,0.,1.));
#11964=DIRECTION('ref_axis',(1.,0.,0.));
#11965=DIRECTION('center_axis',(0.,0.,1.));
#11966=DIRECTION('ref_axis',(1.,0.,0.));
#11967=DIRECTION('center_axis',(0.,0.,1.));
#11968=DIRECTION('ref_axis',(1.,0.,0.));
#11969=DIRECTION('center_axis',(0.,0.,-1.));
#11970=DIRECTION('ref_axis',(1.,0.,0.));
#11971=DIRECTION('center_axis',(0.,0.,1.));
#11972=DIRECTION('ref_axis',(1.,0.,0.));
#11973=DIRECTION('',(0.,0.,-1.));
#11974=DIRECTION('center_axis',(0.,0.,1.));
#11975=DIRECTION('ref_axis',(1.,0.,0.));
#11976=DIRECTION('',(0.,0.,-1.));
#11977=DIRECTION('center_axis',(0.,0.,1.));
#11978=DIRECTION('ref_axis',(1.,0.,0.));
#11979=DIRECTION('center_axis',(0.,0.,1.));
#11980=DIRECTION('ref_axis',(1.,0.,0.));
#11981=DIRECTION('axis',(0.,0.,1.));
#11982=DIRECTION('refdir',(1.,0.,0.));
#11983=DIRECTION('center_axis',(0.,0.,1.));
#11984=DIRECTION('ref_axis',(1.,0.,0.));
#11985=DIRECTION('center_axis',(0.,0.,1.));
#11986=DIRECTION('ref_axis',(1.,0.,0.));
#11987=DIRECTION('',(0.,0.,1.));
#11988=DIRECTION('center_axis',(0.,0.,1.));
#11989=DIRECTION('ref_axis',(1.,0.,0.));
#11990=DIRECTION('center_axis',(0.,0.,1.));
#11991=DIRECTION('ref_axis',(1.,0.,0.));
#11992=DIRECTION('center_axis',(0.,0.,1.));
#11993=DIRECTION('ref_axis',(1.,0.,0.));
#11994=DIRECTION('center_axis',(0.,0.,1.));
#11995=DIRECTION('ref_axis',(1.,0.,0.));
#11996=DIRECTION('',(0.,0.,-1.));
#11997=DIRECTION('center_axis',(0.,0.,1.));
#11998=DIRECTION('ref_axis',(1.,0.,0.));
#11999=DIRECTION('center_axis',(0.,0.,1.));
#12000=DIRECTION('ref_axis',(1.,0.,0.));
#12001=DIRECTION('center_axis',(0.,0.,1.));
#12002=DIRECTION('ref_axis',(1.,0.,0.));
#12003=DIRECTION('axis',(0.,0.,1.));
#12004=DIRECTION('refdir',(1.,0.,0.));
#12005=DIRECTION('center_axis',(0.,0.,1.));
#12006=DIRECTION('ref_axis',(1.,0.,0.));
#12007=DIRECTION('center_axis',(0.,0.,-1.));
#12008=DIRECTION('ref_axis',(1.,0.,0.));
#12009=DIRECTION('',(0.,0.,-1.));
#12010=DIRECTION('center_axis',(0.,0.,-1.));
#12011=DIRECTION('ref_axis',(1.,0.,0.));
#12012=DIRECTION('center_axis',(0.,0.,1.));
#12013=DIRECTION('ref_axis',(1.,0.,0.));
#12014=DIRECTION('center_axis',(0.,0.,1.));
#12015=DIRECTION('ref_axis',(1.,0.,0.));
#12016=DIRECTION('',(0.,0.,-1.));
#12017=DIRECTION('center_axis',(0.,0.,1.));
#12018=DIRECTION('ref_axis',(1.,0.,0.));
#12019=DIRECTION('center_axis',(0.,0.,1.));
#12020=DIRECTION('ref_axis',(1.,0.,0.));
#12021=DIRECTION('center_axis',(0.,0.,1.));
#12022=DIRECTION('ref_axis',(1.,0.,0.));
#12023=DIRECTION('axis',(0.,0.,1.));
#12024=DIRECTION('refdir',(1.,0.,0.));
#12025=DIRECTION('center_axis',(1.,0.,0.));
#12026=DIRECTION('ref_axis',(0.,0.,-1.));
#12027=DIRECTION('',(0.,0.,1.));
#12028=DIRECTION('center_axis',(1.,0.,0.));
#12029=DIRECTION('ref_axis',(0.,0.,-1.));
#12030=DIRECTION('center_axis',(1.,0.,0.));
#12031=DIRECTION('ref_axis',(0.,0.,-1.));
#12032=DIRECTION('center_axis',(1.,0.,0.));
#12033=DIRECTION('ref_axis',(0.,0.,-1.));
#12034=DIRECTION('',(1.,0.,0.));
#12035=DIRECTION('center_axis',(1.,0.,0.));
#12036=DIRECTION('ref_axis',(0.,0.,-1.));
#12037=DIRECTION('',(0.,0.,-1.));
#12038=DIRECTION('center_axis',(0.,0.,1.));
#12039=DIRECTION('ref_axis',(1.,0.,0.));
#12040=DIRECTION('center_axis',(0.,0.,-1.));
#12041=DIRECTION('ref_axis',(1.,0.,0.));
#12042=DIRECTION('',(0.,0.,-1.));
#12043=DIRECTION('center_axis',(0.,0.,-1.));
#12044=DIRECTION('ref_axis',(1.,0.,0.));
#12045=DIRECTION('center_axis',(0.,0.,1.));
#12046=DIRECTION('ref_axis',(1.,0.,0.));
#12047=DIRECTION('center_axis',(0.,0.,1.));
#12048=DIRECTION('ref_axis',(1.,0.,0.));
#12049=DIRECTION('',(0.,0.,-1.));
#12050=DIRECTION('center_axis',(0.,0.,1.));
#12051=DIRECTION('ref_axis',(1.,0.,0.));
#12052=DIRECTION('center_axis',(0.,0.,1.));
#12053=DIRECTION('ref_axis',(1.,0.,0.));
#12054=DIRECTION('center_axis',(0.,0.,1.));
#12055=DIRECTION('ref_axis',(1.,0.,0.));
#12056=DIRECTION('axis',(0.,0.,1.));
#12057=DIRECTION('refdir',(1.,0.,0.));
#12058=DIRECTION('center_axis',(0.,0.,1.));
#12059=DIRECTION('ref_axis',(1.,0.,0.));
#12060=DIRECTION('center_axis',(0.,0.,1.));
#12061=DIRECTION('ref_axis',(1.,0.,0.));
#12062=DIRECTION('',(0.,0.,1.));
#12063=DIRECTION('center_axis',(0.,0.,-1.));
#12064=DIRECTION('ref_axis',(1.,0.,0.));
#12065=DIRECTION('center_axis',(0.,0.,1.));
#12066=DIRECTION('ref_axis',(1.,0.,0.));
#12067=DIRECTION('center_axis',(0.,0.,1.));
#12068=DIRECTION('ref_axis',(1.,0.,0.));
#12069=DIRECTION('center_axis',(0.,0.,1.));
#12070=DIRECTION('ref_axis',(1.,0.,0.));
#12071=DIRECTION('center_axis',(0.,0.,1.));
#12072=DIRECTION('ref_axis',(1.,0.,0.));
#12073=DIRECTION('center_axis',(0.,0.,1.));
#12074=DIRECTION('ref_axis',(1.,0.,0.));
#12075=DIRECTION('center_axis',(0.,0.,1.));
#12076=DIRECTION('ref_axis',(1.,0.,0.));
#12077=DIRECTION('center_axis',(0.,0.,-1.));
#12078=DIRECTION('ref_axis',(1.,0.,0.));
#12079=DIRECTION('center_axis',(0.,0.,1.));
#12080=DIRECTION('ref_axis',(1.,0.,0.));
#12081=DIRECTION('',(0.,0.,-1.));
#12082=DIRECTION('center_axis',(0.,0.,1.));
#12083=DIRECTION('ref_axis',(1.,0.,0.));
#12084=DIRECTION('',(0.,0.,-1.));
#12085=DIRECTION('center_axis',(0.,0.,1.));
#12086=DIRECTION('ref_axis',(1.,0.,0.));
#12087=DIRECTION('center_axis',(0.,0.,1.));
#12088=DIRECTION('ref_axis',(1.,0.,0.));
#12089=DIRECTION('center_axis',(0.,0.,1.));
#12090=DIRECTION('ref_axis',(1.,0.,0.));
#12091=DIRECTION('',(0.,0.,-1.));
#12092=DIRECTION('center_axis',(0.,0.,1.));
#12093=DIRECTION('ref_axis',(1.,0.,0.));
#12094=DIRECTION('center_axis',(0.,0.,1.));
#12095=DIRECTION('ref_axis',(1.,0.,0.));
#12096=DIRECTION('axis',(0.,0.,1.));
#12097=DIRECTION('refdir',(1.,0.,0.));
#12098=DIRECTION('center_axis',(0.,0.,1.));
#12099=DIRECTION('ref_axis',(1.,0.,0.));
#12100=DIRECTION('center_axis',(0.,0.,-1.));
#12101=DIRECTION('ref_axis',(1.,0.,0.));
#12102=DIRECTION('',(0.,0.,-1.));
#12103=DIRECTION('center_axis',(0.,0.,-1.));
#12104=DIRECTION('ref_axis',(1.,0.,0.));
#12105=DIRECTION('center_axis',(0.,0.,1.));
#12106=DIRECTION('ref_axis',(1.,0.,0.));
#12107=DIRECTION('center_axis',(0.,0.,1.));
#12108=DIRECTION('ref_axis',(1.,0.,0.));
#12109=DIRECTION('',(0.,0.,-1.));
#12110=DIRECTION('center_axis',(0.,0.,1.));
#12111=DIRECTION('ref_axis',(1.,0.,0.));
#12112=DIRECTION('center_axis',(0.,0.,1.));
#12113=DIRECTION('ref_axis',(1.,0.,0.));
#12114=DIRECTION('center_axis',(0.,0.,1.));
#12115=DIRECTION('ref_axis',(1.,0.,0.));
#12116=DIRECTION('axis',(0.,0.,1.));
#12117=DIRECTION('refdir',(1.,0.,0.));
#12118=DIRECTION('center_axis',(0.,0.,1.));
#12119=DIRECTION('ref_axis',(1.,0.,0.));
#12120=DIRECTION('center_axis',(0.,0.,-1.));
#12121=DIRECTION('ref_axis',(1.,0.,0.));
#12122=DIRECTION('',(0.,0.,-1.));
#12123=DIRECTION('center_axis',(0.,0.,-1.));
#12124=DIRECTION('ref_axis',(1.,0.,0.));
#12125=DIRECTION('center_axis',(0.,0.,1.));
#12126=DIRECTION('ref_axis',(1.,0.,0.));
#12127=DIRECTION('center_axis',(0.,0.,1.));
#12128=DIRECTION('ref_axis',(1.,0.,0.));
#12129=DIRECTION('',(0.,0.,-1.));
#12130=DIRECTION('center_axis',(0.,0.,1.));
#12131=DIRECTION('ref_axis',(1.,0.,0.));
#12132=DIRECTION('center_axis',(0.,0.,1.));
#12133=DIRECTION('ref_axis',(1.,0.,0.));
#12134=DIRECTION('center_axis',(0.,0.,1.));
#12135=DIRECTION('ref_axis',(1.,0.,0.));
#12136=DIRECTION('axis',(0.,0.,1.));
#12137=DIRECTION('refdir',(1.,0.,0.));
#12138=DIRECTION('center_axis',(0.,0.,1.));
#12139=DIRECTION('ref_axis',(1.,0.,0.));
#12140=DIRECTION('center_axis',(0.,0.,-1.));
#12141=DIRECTION('ref_axis',(1.,0.,0.));
#12142=DIRECTION('',(0.,0.,-1.));
#12143=DIRECTION('center_axis',(0.,0.,-1.));
#12144=DIRECTION('ref_axis',(1.,0.,0.));
#12145=DIRECTION('center_axis',(0.,0.,1.));
#12146=DIRECTION('ref_axis',(1.,0.,0.));
#12147=DIRECTION('center_axis',(0.,0.,1.));
#12148=DIRECTION('ref_axis',(1.,0.,0.));
#12149=DIRECTION('',(0.,0.,-1.));
#12150=DIRECTION('center_axis',(0.,0.,1.));
#12151=DIRECTION('ref_axis',(1.,0.,0.));
#12152=DIRECTION('center_axis',(0.,0.,1.));
#12153=DIRECTION('ref_axis',(1.,0.,0.));
#12154=DIRECTION('center_axis',(0.,0.,1.));
#12155=DIRECTION('ref_axis',(1.,0.,0.));
#12156=DIRECTION('axis',(0.,0.,1.));
#12157=DIRECTION('refdir',(1.,0.,0.));
#12158=DIRECTION('center_axis',(0.,0.,1.));
#12159=DIRECTION('ref_axis',(1.,0.,0.));
#12160=DIRECTION('center_axis',(0.,0.,1.));
#12161=DIRECTION('ref_axis',(1.,0.,0.));
#12162=DIRECTION('',(0.,0.,1.));
#12163=DIRECTION('center_axis',(0.,0.,-1.));
#12164=DIRECTION('ref_axis',(1.,0.,0.));
#12165=DIRECTION('center_axis',(0.,0.,1.));
#12166=DIRECTION('ref_axis',(1.,0.,0.));
#12167=DIRECTION('center_axis',(0.,0.,1.));
#12168=DIRECTION('ref_axis',(1.,0.,0.));
#12169=DIRECTION('center_axis',(0.,0.,1.));
#12170=DIRECTION('ref_axis',(1.,0.,0.));
#12171=DIRECTION('center_axis',(0.,0.,1.));
#12172=DIRECTION('ref_axis',(1.,0.,0.));
#12173=DIRECTION('center_axis',(0.,0.,1.));
#12174=DIRECTION('ref_axis',(1.,0.,0.));
#12175=DIRECTION('center_axis',(0.,0.,1.));
#12176=DIRECTION('ref_axis',(1.,0.,0.));
#12177=DIRECTION('center_axis',(0.,0.,-1.));
#12178=DIRECTION('ref_axis',(1.,0.,0.));
#12179=DIRECTION('center_axis',(0.,0.,1.));
#12180=DIRECTION('ref_axis',(1.,0.,0.));
#12181=DIRECTION('',(0.,0.,-1.));
#12182=DIRECTION('center_axis',(0.,0.,1.));
#12183=DIRECTION('ref_axis',(1.,0.,0.));
#12184=DIRECTION('',(0.,0.,-1.));
#12185=DIRECTION('center_axis',(0.,0.,1.));
#12186=DIRECTION('ref_axis',(1.,0.,0.));
#12187=DIRECTION('center_axis',(0.,0.,1.));
#12188=DIRECTION('ref_axis',(1.,0.,0.));
#12189=DIRECTION('center_axis',(0.,0.,1.));
#12190=DIRECTION('ref_axis',(1.,0.,0.));
#12191=DIRECTION('',(0.,0.,-1.));
#12192=DIRECTION('center_axis',(0.,0.,1.));
#12193=DIRECTION('ref_axis',(1.,0.,0.));
#12194=DIRECTION('center_axis',(0.,0.,1.));
#12195=DIRECTION('ref_axis',(1.,0.,0.));
#12196=DIRECTION('axis',(0.,0.,1.));
#12197=DIRECTION('refdir',(1.,0.,0.));
#12198=DIRECTION('center_axis',(0.,0.,1.));
#12199=DIRECTION('ref_axis',(1.,0.,0.));
#12200=DIRECTION('center_axis',(0.,0.,-1.));
#12201=DIRECTION('ref_axis',(1.,0.,0.));
#12202=DIRECTION('',(0.,0.,-1.));
#12203=DIRECTION('center_axis',(0.,0.,-1.));
#12204=DIRECTION('ref_axis',(1.,0.,0.));
#12205=DIRECTION('center_axis',(0.,0.,1.));
#12206=DIRECTION('ref_axis',(1.,0.,0.));
#12207=DIRECTION('center_axis',(0.,0.,1.));
#12208=DIRECTION('ref_axis',(1.,0.,0.));
#12209=DIRECTION('',(0.,0.,-1.));
#12210=DIRECTION('center_axis',(0.,0.,1.));
#12211=DIRECTION('ref_axis',(1.,0.,0.));
#12212=DIRECTION('center_axis',(0.,0.,1.));
#12213=DIRECTION('ref_axis',(1.,0.,0.));
#12214=DIRECTION('center_axis',(0.,0.,1.));
#12215=DIRECTION('ref_axis',(1.,0.,0.));
#12216=DIRECTION('axis',(0.,0.,1.));
#12217=DIRECTION('refdir',(1.,0.,0.));
#12218=DIRECTION('center_axis',(0.,0.,1.));
#12219=DIRECTION('ref_axis',(1.,0.,0.));
#12220=DIRECTION('center_axis',(0.,0.,-1.));
#12221=DIRECTION('ref_axis',(1.,0.,0.));
#12222=DIRECTION('',(0.,0.,-1.));
#12223=DIRECTION('center_axis',(0.,0.,-1.));
#12224=DIRECTION('ref_axis',(1.,0.,0.));
#12225=DIRECTION('center_axis',(0.,0.,1.));
#12226=DIRECTION('ref_axis',(1.,0.,0.));
#12227=DIRECTION('center_axis',(0.,0.,1.));
#12228=DIRECTION('ref_axis',(1.,0.,0.));
#12229=DIRECTION('',(0.,0.,-1.));
#12230=DIRECTION('center_axis',(0.,0.,1.));
#12231=DIRECTION('ref_axis',(1.,0.,0.));
#12232=DIRECTION('center_axis',(0.,0.,1.));
#12233=DIRECTION('ref_axis',(1.,0.,0.));
#12234=DIRECTION('center_axis',(0.,0.,1.));
#12235=DIRECTION('ref_axis',(1.,0.,0.));
#12236=DIRECTION('axis',(0.,0.,1.));
#12237=DIRECTION('refdir',(1.,0.,0.));
#12238=DIRECTION('center_axis',(0.,0.,1.));
#12239=DIRECTION('ref_axis',(1.,0.,0.));
#12240=DIRECTION('center_axis',(0.,0.,-1.));
#12241=DIRECTION('ref_axis',(1.,0.,0.));
#12242=DIRECTION('',(0.,0.,-1.));
#12243=DIRECTION('center_axis',(0.,0.,-1.));
#12244=DIRECTION('ref_axis',(1.,0.,0.));
#12245=DIRECTION('center_axis',(0.,0.,1.));
#12246=DIRECTION('ref_axis',(1.,0.,0.));
#12247=DIRECTION('center_axis',(0.,0.,1.));
#12248=DIRECTION('ref_axis',(1.,0.,0.));
#12249=DIRECTION('',(0.,0.,-1.));
#12250=DIRECTION('center_axis',(0.,0.,1.));
#12251=DIRECTION('ref_axis',(1.,0.,0.));
#12252=DIRECTION('center_axis',(0.,0.,1.));
#12253=DIRECTION('ref_axis',(1.,0.,0.));
#12254=DIRECTION('center_axis',(0.,0.,1.));
#12255=DIRECTION('ref_axis',(1.,0.,0.));
#12256=DIRECTION('axis',(0.,0.,1.));
#12257=DIRECTION('refdir',(1.,0.,0.));
#12258=DIRECTION('center_axis',(0.,1.,0.));
#12259=DIRECTION('ref_axis',(0.,0.,1.));
#12260=DIRECTION('center_axis',(0.,-1.,0.));
#12261=DIRECTION('ref_axis',(1.,0.,0.));
#12262=DIRECTION('center_axis',(0.,-1.,0.));
#12263=DIRECTION('ref_axis',(1.,0.,0.));
#12264=DIRECTION('center_axis',(0.,-1.,0.));
#12265=DIRECTION('ref_axis',(1.,0.,0.));
#12266=DIRECTION('',(0.707106781186547,0.707106781186548,8.65956056235493E-17));
#12267=DIRECTION('center_axis',(0.,-1.,0.));
#12268=DIRECTION('ref_axis',(1.,0.,0.));
#12269=DIRECTION('center_axis',(0.,-1.,0.));
#12270=DIRECTION('ref_axis',(1.,0.,0.));
#12271=DIRECTION('',(0.,1.,0.));
#12272=DIRECTION('center_axis',(0.,1.,0.));
#12273=DIRECTION('ref_axis',(1.,0.,0.));
#12274=DIRECTION('center_axis',(0.,-1.,0.));
#12275=DIRECTION('ref_axis',(1.,0.,0.));
#12276=DIRECTION('',(-0.707106781186547,0.707106781186548,-8.65956056235493E-17));
#12277=DIRECTION('center_axis',(0.,-1.,0.));
#12278=DIRECTION('ref_axis',(0.,0.,-1.));
#12279=DIRECTION('center_axis',(0.,-1.,0.));
#12280=DIRECTION('ref_axis',(1.,0.,0.));
#12281=DIRECTION('center_axis',(0.,1.,0.));
#12282=DIRECTION('ref_axis',(1.,0.,0.));
#12283=DIRECTION('center_axis',(0.,1.,0.));
#12284=DIRECTION('ref_axis',(1.,0.,0.));
#12285=DIRECTION('',(-0.447213595499958,0.894427190999916,-5.47678698264203E-17));
#12286=DIRECTION('center_axis',(0.,-1.,0.));
#12287=DIRECTION('ref_axis',(1.,0.,0.));
#12288=DIRECTION('center_axis',(0.,1.,0.));
#12289=DIRECTION('ref_axis',(1.,0.,0.));
#12290=DIRECTION('',(0.,1.,0.));
#12291=DIRECTION('center_axis',(0.,1.,0.));
#12292=DIRECTION('ref_axis',(1.,0.,0.));
#12293=DIRECTION('center_axis',(0.,-1.,0.));
#12294=DIRECTION('ref_axis',(1.,0.,0.));
#12295=DIRECTION('',(-0.707106781186547,0.707106781186548,-8.65956056235493E-17));
#12296=DIRECTION('center_axis',(0.,-1.,0.));
#12297=DIRECTION('ref_axis',(0.,0.,-1.));
#12298=DIRECTION('center_axis',(0.866025403784439,0.,-0.5));
#12299=DIRECTION('ref_axis',(0.5,0.,0.866025403784439));
#12300=DIRECTION('',(-0.5,0.,-0.866025403784439));
#12301=DIRECTION('',(0.,-1.,0.));
#12302=DIRECTION('',(0.5,0.,0.866025403784439));
#12303=DIRECTION('',(0.,-1.,0.));
#12304=DIRECTION('center_axis',(1.60246890531964E-16,0.,-1.));
#12305=DIRECTION('ref_axis',(1.,0.,1.60246890531964E-16));
#12306=DIRECTION('',(-1.,0.,-1.60246890531964E-16));
#12307=DIRECTION('',(0.,-1.,0.));
#12308=DIRECTION('',(1.,0.,1.60246890531964E-16));
#12309=DIRECTION('center_axis',(-0.866025403784439,0.,-0.5));
#12310=DIRECTION('ref_axis',(0.5,0.,-0.866025403784439));
#12311=DIRECTION('',(-0.5,0.,0.866025403784439));
#12312=DIRECTION('',(0.,-1.,0.));
#12313=DIRECTION('',(0.5,0.,-0.866025403784439));
#12314=DIRECTION('center_axis',(-0.866025403784439,0.,0.5));
#12315=DIRECTION('ref_axis',(-0.5,0.,-0.866025403784439));
#12316=DIRECTION('',(0.5,0.,0.866025403784439));
#12317=DIRECTION('',(0.,-1.,0.));
#12318=DIRECTION('',(-0.5,0.,-0.866025403784439));
#12319=DIRECTION('center_axis',(-1.60246890531964E-16,0.,1.));
#12320=DIRECTION('ref_axis',(-1.,0.,-1.60246890531964E-16));
#12321=DIRECTION('',(1.,0.,1.60246890531964E-16));
#12322=DIRECTION('',(0.,-1.,0.));
#12323=DIRECTION('',(-1.,0.,-1.60246890531964E-16));
#12324=DIRECTION('center_axis',(0.866025403784439,0.,0.5));
#12325=DIRECTION('ref_axis',(-0.5,0.,0.866025403784439));
#12326=DIRECTION('',(0.5,0.,-0.866025403784439));
#12327=DIRECTION('',(-0.5,0.,0.866025403784439));
#12328=DIRECTION('center_axis',(0.,1.,0.));
#12329=DIRECTION('ref_axis',(1.,0.,0.));
#12330=DIRECTION('center_axis',(0.,-1.,0.));
#12331=DIRECTION('ref_axis',(0.,0.,-1.));
#12332=DIRECTION('axis',(0.,0.,1.));
#12333=DIRECTION('refdir',(1.,0.,0.));
#12334=DIRECTION('center_axis',(0.,1.,0.));
#12335=DIRECTION('ref_axis',(1.,0.,0.));
#12336=DIRECTION('center_axis',(0.,1.,0.));
#12337=DIRECTION('ref_axis',(1.,0.,0.));
#12338=DIRECTION('center_axis',(0.866025403784439,0.,-0.5));
#12339=DIRECTION('ref_axis',(0.5,0.,0.866025403784439));
#12340=DIRECTION('',(0.5,0.,0.866025403784439));
#12341=DIRECTION('',(0.,-1.,0.));
#12342=DIRECTION('',(0.5,0.,0.866025403784439));
#12343=DIRECTION('',(0.,-1.,0.));
#12344=DIRECTION('center_axis',(1.20185167898973E-16,0.,-1.));
#12345=DIRECTION('ref_axis',(1.,0.,1.20185167898973E-16));
#12346=DIRECTION('',(1.,0.,1.20185167898973E-16));
#12347=DIRECTION('',(0.,-1.,0.));
#12348=DIRECTION('',(1.,0.,1.20185167898973E-16));
#12349=DIRECTION('center_axis',(-0.866025403784439,0.,-0.5));
#12350=DIRECTION('ref_axis',(0.5,0.,-0.866025403784439));
#12351=DIRECTION('',(0.5,0.,-0.866025403784439));
#12352=DIRECTION('',(0.,-1.,0.));
#12353=DIRECTION('',(0.5,0.,-0.866025403784439));
#12354=DIRECTION('center_axis',(-0.866025403784439,0.,0.5));
#12355=DIRECTION('ref_axis',(-0.5,0.,-0.866025403784439));
#12356=DIRECTION('',(-0.5,0.,-0.866025403784439));
#12357=DIRECTION('',(0.,-1.,0.));
#12358=DIRECTION('',(-0.5,0.,-0.866025403784439));
#12359=DIRECTION('center_axis',(-2.40370335797945E-16,0.,1.));
#12360=DIRECTION('ref_axis',(-1.,0.,-2.40370335797945E-16));
#12361=DIRECTION('',(-1.,0.,-2.40370335797945E-16));
#12362=DIRECTION('',(0.,-1.,0.));
#12363=DIRECTION('',(-1.,0.,-2.40370335797945E-16));
#12364=DIRECTION('center_axis',(0.866025403784439,0.,0.5));
#12365=DIRECTION('ref_axis',(-0.5,0.,0.866025403784439));
#12366=DIRECTION('',(-0.5,0.,0.866025403784439));
#12367=DIRECTION('',(-0.5,0.,0.866025403784439));
#12368=DIRECTION('center_axis',(0.,-1.,0.));
#12369=DIRECTION('ref_axis',(0.,0.,-1.));
#12370=DIRECTION('center_axis',(0.,1.,0.));
#12371=DIRECTION('ref_axis',(0.,0.,1.));
#12372=DIRECTION('center_axis',(0.,-1.,0.));
#12373=DIRECTION('ref_axis',(1.,0.,0.));
#12374=DIRECTION('center_axis',(0.,-1.,0.));
#12375=DIRECTION('ref_axis',(1.,0.,0.));
#12376=DIRECTION('center_axis',(0.,-1.,0.));
#12377=DIRECTION('ref_axis',(1.,0.,0.));
#12378=DIRECTION('',(0.707106781186548,0.707106781186547,8.65956056235494E-17));
#12379=DIRECTION('center_axis',(0.,-1.,0.));
#12380=DIRECTION('ref_axis',(1.,0.,0.));
#12381=DIRECTION('',(0.,1.,0.));
#12382=DIRECTION('axis',(0.,0.,1.));
#12383=DIRECTION('refdir',(1.,0.,0.));
#12384=DIRECTION('axis',(0.,0.,1.));
#12385=DIRECTION('refdir',(1.,0.,0.));
#12386=DIRECTION('center_axis',(0.,0.,1.));
#12387=DIRECTION('ref_axis',(1.,0.,0.));
#12388=DIRECTION('center_axis',(0.,0.,1.));
#12389=DIRECTION('ref_axis',(1.,0.,0.));
#12390=DIRECTION('',(0.,0.,1.));
#12391=DIRECTION('center_axis',(0.,0.,-1.));
#12392=DIRECTION('ref_axis',(1.,0.,0.));
#12393=DIRECTION('center_axis',(0.,0.,1.));
#12394=DIRECTION('ref_axis',(1.,0.,0.));
#12395=DIRECTION('center_axis',(0.,0.,1.));
#12396=DIRECTION('ref_axis',(1.,0.,0.));
#12397=DIRECTION('',(0.,0.,1.));
#12398=DIRECTION('center_axis',(0.,0.,-1.));
#12399=DIRECTION('ref_axis',(1.,0.,0.));
#12400=DIRECTION('center_axis',(0.,0.,1.));
#12401=DIRECTION('ref_axis',(1.,0.,0.));
#12402=DIRECTION('',(0.,0.,-1.));
#12403=DIRECTION('center_axis',(0.,0.,1.));
#12404=DIRECTION('ref_axis',(1.,0.,0.));
#12405=DIRECTION('',(0.,0.,1.));
#12406=DIRECTION('center_axis',(0.,0.,1.));
#12407=DIRECTION('ref_axis',(1.,0.,0.));
#12408=DIRECTION('center_axis',(0.,1.,0.));
#12409=DIRECTION('ref_axis',(-1.,0.,0.));
#12410=DIRECTION('',(1.,0.,0.));
#12411=DIRECTION('',(0.,0.,-1.));
#12412=DIRECTION('',(-1.,0.,0.));
#12413=DIRECTION('center_axis',(0.,0.,1.));
#12414=DIRECTION('ref_axis',(1.,0.,0.));
#12415=DIRECTION('',(-1.,0.,0.));
#12416=DIRECTION('center_axis',(0.,0.,1.));
#12417=DIRECTION('ref_axis',(1.,0.,0.));
#12418=DIRECTION('center_axis',(0.,-1.,0.));
#12419=DIRECTION('ref_axis',(1.,0.,0.));
#12420=DIRECTION('',(1.,0.,0.));
#12421=DIRECTION('',(0.,0.,1.));
#12422=DIRECTION('center_axis',(0.,0.,1.));
#12423=DIRECTION('ref_axis',(-1.,1.22464679914735E-16,0.));
#12424=DIRECTION('center_axis',(0.,0.,1.));
#12425=DIRECTION('ref_axis',(1.,0.,0.));
#12426=DIRECTION('center_axis',(0.,0.,1.));
#12427=DIRECTION('ref_axis',(1.,0.,0.));
#12428=DIRECTION('axis',(0.,0.,1.));
#12429=DIRECTION('refdir',(1.,0.,0.));
#12430=DIRECTION('center_axis',(0.,0.,1.));
#12431=DIRECTION('ref_axis',(1.,0.,0.));
#12432=DIRECTION('center_axis',(0.,0.,-1.));
#12433=DIRECTION('ref_axis',(1.,0.,0.));
#12434=DIRECTION('',(0.,0.,-1.));
#12435=DIRECTION('center_axis',(0.,0.,-1.));
#12436=DIRECTION('ref_axis',(1.,0.,0.));
#12437=DIRECTION('center_axis',(0.,0.,1.));
#12438=DIRECTION('ref_axis',(1.,0.,0.));
#12439=DIRECTION('center_axis',(0.,0.,1.));
#12440=DIRECTION('ref_axis',(1.,0.,0.));
#12441=DIRECTION('',(0.,0.,-1.));
#12442=DIRECTION('center_axis',(0.,0.,1.));
#12443=DIRECTION('ref_axis',(1.,0.,0.));
#12444=DIRECTION('center_axis',(0.,0.,1.));
#12445=DIRECTION('ref_axis',(1.,0.,0.));
#12446=DIRECTION('center_axis',(0.,0.,1.));
#12447=DIRECTION('ref_axis',(1.,0.,0.));
#12448=DIRECTION('axis',(0.,0.,1.));
#12449=DIRECTION('refdir',(1.,0.,0.));
#12450=DIRECTION('center_axis',(0.,0.,1.));
#12451=DIRECTION('ref_axis',(1.,0.,0.));
#12452=DIRECTION('center_axis',(0.,0.,-1.));
#12453=DIRECTION('ref_axis',(1.,0.,0.));
#12454=DIRECTION('',(0.,0.,-1.));
#12455=DIRECTION('center_axis',(0.,0.,-1.));
#12456=DIRECTION('ref_axis',(1.,0.,0.));
#12457=DIRECTION('center_axis',(0.,0.,1.));
#12458=DIRECTION('ref_axis',(1.,0.,0.));
#12459=DIRECTION('center_axis',(0.,0.,1.));
#12460=DIRECTION('ref_axis',(1.,0.,0.));
#12461=DIRECTION('',(0.,0.,-1.));
#12462=DIRECTION('center_axis',(0.,0.,1.));
#12463=DIRECTION('ref_axis',(1.,0.,0.));
#12464=DIRECTION('center_axis',(0.,0.,1.));
#12465=DIRECTION('ref_axis',(1.,0.,0.));
#12466=DIRECTION('center_axis',(0.,0.,1.));
#12467=DIRECTION('ref_axis',(1.,0.,0.));
#12468=DIRECTION('',(0.,0.,1.));
#12469=DIRECTION('',(1.,0.,0.));
#12470=DIRECTION('',(0.,0.,1.));
#12471=DIRECTION('',(1.,0.,0.));
#12472=DIRECTION('',(0.,0.,1.));
#12473=DIRECTION('',(1.,0.,0.));
#12474=DIRECTION('axis',(0.,0.,1.));
#12475=DIRECTION('refdir',(1.,0.,0.));
#12476=DIRECTION('axis',(0.,0.,1.));
#12477=DIRECTION('refdir',(1.,0.,0.));
#12478=DIRECTION('center_axis',(0.,0.,1.));
#12479=DIRECTION('ref_axis',(1.,0.,0.));
#12480=DIRECTION('center_axis',(0.,0.,1.));
#12481=DIRECTION('ref_axis',(1.,0.,0.));
#12482=DIRECTION('',(0.,0.,1.));
#12483=DIRECTION('center_axis',(0.,0.,-1.));
#12484=DIRECTION('ref_axis',(1.,0.,0.));
#12485=DIRECTION('center_axis',(0.,0.,1.));
#12486=DIRECTION('ref_axis',(1.,0.,0.));
#12487=DIRECTION('center_axis',(0.,0.,1.));
#12488=DIRECTION('ref_axis',(1.,0.,0.));
#12489=DIRECTION('',(0.,0.,1.));
#12490=DIRECTION('center_axis',(0.,0.,-1.));
#12491=DIRECTION('ref_axis',(1.,0.,0.));
#12492=DIRECTION('center_axis',(0.,0.,1.));
#12493=DIRECTION('ref_axis',(-1.83697019872103E-16,1.,0.));
#12494=DIRECTION('',(0.,0.,-1.));
#12495=DIRECTION('center_axis',(0.,0.,1.));
#12496=DIRECTION('ref_axis',(1.,0.,0.));
#12497=DIRECTION('',(0.,0.,1.));
#12498=DIRECTION('center_axis',(0.,0.,1.));
#12499=DIRECTION('ref_axis',(1.,0.,0.));
#12500=DIRECTION('center_axis',(-1.,0.,0.));
#12501=DIRECTION('ref_axis',(0.,-1.,0.));
#12502=DIRECTION('',(0.,1.,0.));
#12503=DIRECTION('',(0.,0.,-1.));
#12504=DIRECTION('',(0.,-1.,0.));
#12505=DIRECTION('center_axis',(0.,0.,1.));
#12506=DIRECTION('ref_axis',(1.,0.,0.));
#12507=DIRECTION('',(0.,-1.,0.));
#12508=DIRECTION('center_axis',(0.,0.,1.));
#12509=DIRECTION('ref_axis',(1.,0.,0.));
#12510=DIRECTION('center_axis',(1.,0.,0.));
#12511=DIRECTION('ref_axis',(0.,1.,0.));
#12512=DIRECTION('',(0.,1.,0.));
#12513=DIRECTION('',(0.,0.,1.));
#12514=DIRECTION('center_axis',(0.,0.,1.));
#12515=DIRECTION('ref_axis',(-1.83697019872103E-16,-1.,0.));
#12516=DIRECTION('center_axis',(0.,0.,1.));
#12517=DIRECTION('ref_axis',(1.,0.,0.));
#12518=DIRECTION('center_axis',(0.,0.,1.));
#12519=DIRECTION('ref_axis',(1.,0.,0.));
#12520=DIRECTION('axis',(0.,0.,1.));
#12521=DIRECTION('refdir',(1.,0.,0.));
#12522=DIRECTION('center_axis',(0.,0.,1.));
#12523=DIRECTION('ref_axis',(1.,0.,0.));
#12524=DIRECTION('center_axis',(0.,0.,-1.));
#12525=DIRECTION('ref_axis',(1.,0.,0.));
#12526=DIRECTION('',(0.,0.,-1.));
#12527=DIRECTION('center_axis',(0.,0.,-1.));
#12528=DIRECTION('ref_axis',(1.,0.,0.));
#12529=DIRECTION('center_axis',(0.,0.,1.));
#12530=DIRECTION('ref_axis',(1.,0.,0.));
#12531=DIRECTION('center_axis',(0.,0.,1.));
#12532=DIRECTION('ref_axis',(1.,0.,0.));
#12533=DIRECTION('',(0.,0.,-1.));
#12534=DIRECTION('center_axis',(0.,0.,1.));
#12535=DIRECTION('ref_axis',(1.,0.,0.));
#12536=DIRECTION('center_axis',(0.,0.,1.));
#12537=DIRECTION('ref_axis',(1.,0.,0.));
#12538=DIRECTION('center_axis',(0.,0.,1.));
#12539=DIRECTION('ref_axis',(1.,0.,0.));
#12540=DIRECTION('axis',(0.,0.,1.));
#12541=DIRECTION('refdir',(1.,0.,0.));
#12542=DIRECTION('center_axis',(0.,0.,1.));
#12543=DIRECTION('ref_axis',(1.,0.,0.));
#12544=DIRECTION('center_axis',(0.,0.,-1.));
#12545=DIRECTION('ref_axis',(1.,0.,0.));
#12546=DIRECTION('',(0.,0.,-1.));
#12547=DIRECTION('center_axis',(0.,0.,-1.));
#12548=DIRECTION('ref_axis',(1.,0.,0.));
#12549=DIRECTION('center_axis',(0.,0.,1.));
#12550=DIRECTION('ref_axis',(1.,0.,0.));
#12551=DIRECTION('center_axis',(0.,0.,1.));
#12552=DIRECTION('ref_axis',(1.,0.,0.));
#12553=DIRECTION('',(0.,0.,-1.));
#12554=DIRECTION('center_axis',(0.,0.,1.));
#12555=DIRECTION('ref_axis',(1.,0.,0.));
#12556=DIRECTION('center_axis',(0.,0.,1.));
#12557=DIRECTION('ref_axis',(1.,0.,0.));
#12558=DIRECTION('center_axis',(0.,0.,1.));
#12559=DIRECTION('ref_axis',(1.,0.,0.));
#12560=DIRECTION('',(0.,0.,1.));
#12561=DIRECTION('',(1.,0.,0.));
#12562=DIRECTION('',(0.,0.,1.));
#12563=DIRECTION('',(1.,0.,0.));
#12564=DIRECTION('',(0.,0.,1.));
#12565=DIRECTION('',(1.,0.,0.));
#12566=DIRECTION('axis',(0.,0.,1.));
#12567=DIRECTION('refdir',(1.,0.,0.));
#12568=DIRECTION('axis',(0.,0.,1.));
#12569=DIRECTION('refdir',(1.,0.,0.));
#12570=DIRECTION('center_axis',(0.,0.,1.));
#12571=DIRECTION('ref_axis',(1.,0.,0.));
#12572=DIRECTION('center_axis',(0.,0.,1.));
#12573=DIRECTION('ref_axis',(1.,0.,0.));
#12574=DIRECTION('',(0.,0.,1.));
#12575=DIRECTION('center_axis',(0.,0.,-1.));
#12576=DIRECTION('ref_axis',(1.,0.,0.));
#12577=DIRECTION('center_axis',(0.,0.,1.));
#12578=DIRECTION('ref_axis',(1.,0.,0.));
#12579=DIRECTION('center_axis',(1.,0.,0.));
#12580=DIRECTION('ref_axis',(0.,0.,-1.));
#12581=DIRECTION('center_axis',(1.,0.,0.));
#12582=DIRECTION('ref_axis',(0.,0.,-1.));
#12583=DIRECTION('',(1.,0.,0.));
#12584=DIRECTION('center_axis',(-1.,0.,0.));
#12585=DIRECTION('ref_axis',(0.,0.,-1.));
#12586=DIRECTION('center_axis',(1.,0.,0.));
#12587=DIRECTION('ref_axis',(0.,0.,-1.));
#12588=DIRECTION('center_axis',(1.,0.,0.));
#12589=DIRECTION('ref_axis',(0.,0.,-1.));
#12590=DIRECTION('',(1.,0.,0.));
#12591=DIRECTION('center_axis',(-1.,0.,0.));
#12592=DIRECTION('ref_axis',(0.,0.,-1.));
#12593=DIRECTION('center_axis',(1.,0.,0.));
#12594=DIRECTION('ref_axis',(0.,0.,-1.));
#12595=DIRECTION('center_axis',(1.,0.,0.));
#12596=DIRECTION('ref_axis',(0.,0.,-1.));
#12597=DIRECTION('',(1.,0.,0.));
#12598=DIRECTION('center_axis',(-1.,0.,0.));
#12599=DIRECTION('ref_axis',(0.,0.,-1.));
#12600=DIRECTION('center_axis',(1.,0.,0.));
#12601=DIRECTION('ref_axis',(0.,0.,-1.));
#12602=DIRECTION('center_axis',(1.,0.,0.));
#12603=DIRECTION('ref_axis',(0.,0.,-1.));
#12604=DIRECTION('',(1.,0.,0.));
#12605=DIRECTION('center_axis',(-1.,0.,0.));
#12606=DIRECTION('ref_axis',(0.,0.,-1.));
#12607=DIRECTION('center_axis',(1.,0.,0.));
#12608=DIRECTION('ref_axis',(0.,0.,-1.));
#12609=DIRECTION('center_axis',(1.,0.,0.));
#12610=DIRECTION('ref_axis',(0.,0.,-1.));
#12611=DIRECTION('',(1.,0.,0.));
#12612=DIRECTION('center_axis',(-1.,0.,0.));
#12613=DIRECTION('ref_axis',(0.,0.,-1.));
#12614=DIRECTION('center_axis',(0.,1.,0.));
#12615=DIRECTION('ref_axis',(-1.,0.,0.));
#12616=DIRECTION('',(-1.,0.,0.));
#12617=DIRECTION('',(0.,0.,1.));
#12618=DIRECTION('',(-1.,0.,0.));
#12619=DIRECTION('',(0.,0.,1.));
#12620=DIRECTION('center_axis',(1.,0.,0.));
#12621=DIRECTION('ref_axis',(0.,1.,0.));
#12622=DIRECTION('',(0.,1.,0.));
#12623=DIRECTION('',(0.,1.,0.));
#12624=DIRECTION('',(0.,0.,1.));
#12625=DIRECTION('center_axis',(0.,-1.,0.));
#12626=DIRECTION('ref_axis',(1.,0.,0.));
#12627=DIRECTION('',(1.,0.,0.));
#12628=DIRECTION('',(1.,0.,0.));
#12629=DIRECTION('',(0.,0.,1.));
#12630=DIRECTION('center_axis',(-1.,0.,0.));
#12631=DIRECTION('ref_axis',(0.,-1.,0.));
#12632=DIRECTION('',(0.,-1.,0.));
#12633=DIRECTION('',(0.,-1.,0.));
#12634=DIRECTION('center_axis',(0.,0.,1.));
#12635=DIRECTION('ref_axis',(1.,0.,0.));
#12636=DIRECTION('center_axis',(0.,0.,1.));
#12637=DIRECTION('ref_axis',(1.,0.,0.));
#12638=DIRECTION('axis',(0.,0.,1.));
#12639=DIRECTION('refdir',(1.,0.,0.));
#12640=DIRECTION('center_axis',(1.,0.,0.));
#12641=DIRECTION('ref_axis',(0.,0.,-1.));
#12642=DIRECTION('center_axis',(1.,0.,0.));
#12643=DIRECTION('ref_axis',(0.,0.,-1.));
#12644=DIRECTION('',(1.,0.,0.));
#12645=DIRECTION('center_axis',(-1.,0.,0.));
#12646=DIRECTION('ref_axis',(0.,0.,-1.));
#12647=DIRECTION('center_axis',(1.,0.,0.));
#12648=DIRECTION('ref_axis',(0.,0.,-1.));
#12649=DIRECTION('center_axis',(1.,0.,0.));
#12650=DIRECTION('ref_axis',(0.,0.,-1.));
#12651=DIRECTION('',(1.,0.,0.));
#12652=DIRECTION('center_axis',(-1.,0.,0.));
#12653=DIRECTION('ref_axis',(0.,0.,-1.));
#12654=DIRECTION('center_axis',(1.,0.,0.));
#12655=DIRECTION('ref_axis',(0.,0.,-1.));
#12656=DIRECTION('center_axis',(1.,0.,0.));
#12657=DIRECTION('ref_axis',(0.,0.,-1.));
#12658=DIRECTION('',(1.,0.,0.));
#12659=DIRECTION('center_axis',(-1.,0.,0.));
#12660=DIRECTION('ref_axis',(0.,0.,-1.));
#12661=DIRECTION('center_axis',(1.,0.,0.));
#12662=DIRECTION('ref_axis',(0.,0.,-1.));
#12663=DIRECTION('center_axis',(1.,0.,0.));
#12664=DIRECTION('ref_axis',(0.,0.,-1.));
#12665=DIRECTION('',(1.,0.,0.));
#12666=DIRECTION('center_axis',(-1.,0.,0.));
#12667=DIRECTION('ref_axis',(0.,0.,-1.));
#12668=DIRECTION('center_axis',(1.,0.,0.));
#12669=DIRECTION('ref_axis',(0.,0.,-1.));
#12670=DIRECTION('center_axis',(1.,0.,0.));
#12671=DIRECTION('ref_axis',(0.,0.,-1.));
#12672=DIRECTION('',(1.,0.,0.));
#12673=DIRECTION('center_axis',(-1.,0.,0.));
#12674=DIRECTION('ref_axis',(0.,0.,-1.));
#12675=DIRECTION('center_axis',(0.,1.,0.));
#12676=DIRECTION('ref_axis',(-1.,0.,0.));
#12677=DIRECTION('',(-1.,0.,0.));
#12678=DIRECTION('',(0.,0.,1.));
#12679=DIRECTION('',(-1.,0.,0.));
#12680=DIRECTION('',(0.,0.,1.));
#12681=DIRECTION('center_axis',(1.,0.,0.));
#12682=DIRECTION('ref_axis',(0.,1.,0.));
#12683=DIRECTION('',(0.,1.,0.));
#12684=DIRECTION('',(0.,1.,0.));
#12685=DIRECTION('',(0.,0.,1.));
#12686=DIRECTION('center_axis',(0.,-1.,0.));
#12687=DIRECTION('ref_axis',(1.,0.,0.));
#12688=DIRECTION('',(1.,0.,0.));
#12689=DIRECTION('',(1.,0.,0.));
#12690=DIRECTION('',(0.,0.,1.));
#12691=DIRECTION('center_axis',(-1.,0.,0.));
#12692=DIRECTION('ref_axis',(0.,-1.,0.));
#12693=DIRECTION('',(0.,-1.,0.));
#12694=DIRECTION('',(0.,-1.,0.));
#12695=DIRECTION('center_axis',(0.,0.,1.));
#12696=DIRECTION('ref_axis',(1.,0.,0.));
#12697=DIRECTION('center_axis',(0.,0.,1.));
#12698=DIRECTION('ref_axis',(1.,0.,0.));
#12699=DIRECTION('axis',(0.,0.,1.));
#12700=DIRECTION('refdir',(1.,0.,0.));
#12701=DIRECTION('center_axis',(1.,0.,0.));
#12702=DIRECTION('ref_axis',(0.,0.,-1.));
#12703=DIRECTION('center_axis',(1.,0.,0.));
#12704=DIRECTION('ref_axis',(0.,0.,-1.));
#12705=DIRECTION('',(1.,0.,0.));
#12706=DIRECTION('center_axis',(-1.,0.,0.));
#12707=DIRECTION('ref_axis',(0.,0.,-1.));
#12708=DIRECTION('center_axis',(1.,0.,0.));
#12709=DIRECTION('ref_axis',(0.,0.,-1.));
#12710=DIRECTION('center_axis',(1.,0.,0.));
#12711=DIRECTION('ref_axis',(0.,0.,-1.));
#12712=DIRECTION('',(1.,0.,0.));
#12713=DIRECTION('center_axis',(-1.,0.,0.));
#12714=DIRECTION('ref_axis',(0.,0.,-1.));
#12715=DIRECTION('center_axis',(1.,0.,0.));
#12716=DIRECTION('ref_axis',(0.,0.,-1.));
#12717=DIRECTION('center_axis',(1.,0.,0.));
#12718=DIRECTION('ref_axis',(0.,0.,-1.));
#12719=DIRECTION('',(1.,0.,0.));
#12720=DIRECTION('center_axis',(-1.,0.,0.));
#12721=DIRECTION('ref_axis',(0.,0.,-1.));
#12722=DIRECTION('center_axis',(1.,0.,0.));
#12723=DIRECTION('ref_axis',(0.,0.,-1.));
#12724=DIRECTION('center_axis',(1.,0.,0.));
#12725=DIRECTION('ref_axis',(0.,0.,-1.));
#12726=DIRECTION('',(1.,0.,0.));
#12727=DIRECTION('center_axis',(-1.,0.,0.));
#12728=DIRECTION('ref_axis',(0.,0.,-1.));
#12729=DIRECTION('center_axis',(1.,0.,0.));
#12730=DIRECTION('ref_axis',(0.,0.,-1.));
#12731=DIRECTION('center_axis',(1.,0.,0.));
#12732=DIRECTION('ref_axis',(0.,0.,-1.));
#12733=DIRECTION('',(1.,0.,0.));
#12734=DIRECTION('center_axis',(-1.,0.,0.));
#12735=DIRECTION('ref_axis',(0.,0.,-1.));
#12736=DIRECTION('center_axis',(0.,1.,0.));
#12737=DIRECTION('ref_axis',(-1.,0.,0.));
#12738=DIRECTION('',(-1.,0.,0.));
#12739=DIRECTION('',(0.,0.,1.));
#12740=DIRECTION('',(-1.,0.,0.));
#12741=DIRECTION('',(0.,0.,1.));
#12742=DIRECTION('center_axis',(1.,0.,0.));
#12743=DIRECTION('ref_axis',(0.,1.,0.));
#12744=DIRECTION('',(0.,1.,0.));
#12745=DIRECTION('',(0.,1.,0.));
#12746=DIRECTION('',(0.,0.,1.));
#12747=DIRECTION('center_axis',(0.,-1.,0.));
#12748=DIRECTION('ref_axis',(1.,0.,0.));
#12749=DIRECTION('',(1.,0.,0.));
#12750=DIRECTION('',(1.,0.,0.));
#12751=DIRECTION('',(0.,0.,1.));
#12752=DIRECTION('center_axis',(-1.,0.,0.));
#12753=DIRECTION('ref_axis',(0.,-1.,0.));
#12754=DIRECTION('',(0.,-1.,0.));
#12755=DIRECTION('',(0.,-1.,0.));
#12756=DIRECTION('center_axis',(0.,0.,1.));
#12757=DIRECTION('ref_axis',(1.,0.,0.));
#12758=DIRECTION('center_axis',(0.,0.,1.));
#12759=DIRECTION('ref_axis',(1.,0.,0.));
#12760=DIRECTION('axis',(0.,0.,1.));
#12761=DIRECTION('refdir',(1.,0.,0.));
#12762=DIRECTION('center_axis',(0.,0.,1.));
#12763=DIRECTION('ref_axis',(1.,0.,0.));
#12764=DIRECTION('center_axis',(0.,0.,1.));
#12765=DIRECTION('ref_axis',(1.,0.,0.));
#12766=DIRECTION('',(0.,0.,1.));
#12767=DIRECTION('center_axis',(0.,0.,-1.));
#12768=DIRECTION('ref_axis',(1.,0.,0.));
#12769=DIRECTION('center_axis',(0.,0.,1.));
#12770=DIRECTION('ref_axis',(1.,0.,0.));
#12771=DIRECTION('center_axis',(0.,0.,1.));
#12772=DIRECTION('ref_axis',(1.,0.,0.));
#12773=DIRECTION('center_axis',(0.,0.,1.));
#12774=DIRECTION('ref_axis',(1.,0.,0.));
#12775=DIRECTION('center_axis',(0.,0.,1.));
#12776=DIRECTION('ref_axis',(1.,0.,0.));
#12777=DIRECTION('center_axis',(0.,0.,1.));
#12778=DIRECTION('ref_axis',(1.,0.,0.));
#12779=DIRECTION('center_axis',(0.,0.,1.));
#12780=DIRECTION('ref_axis',(1.,0.,0.));
#12781=DIRECTION('center_axis',(0.,0.,-1.));
#12782=DIRECTION('ref_axis',(1.,0.,0.));
#12783=DIRECTION('center_axis',(0.,0.,1.));
#12784=DIRECTION('ref_axis',(1.,0.,0.));
#12785=DIRECTION('',(0.,0.,-1.));
#12786=DIRECTION('center_axis',(0.,0.,1.));
#12787=DIRECTION('ref_axis',(1.,0.,0.));
#12788=DIRECTION('',(0.,0.,-1.));
#12789=DIRECTION('center_axis',(0.,0.,1.));
#12790=DIRECTION('ref_axis',(1.,0.,0.));
#12791=DIRECTION('center_axis',(0.,0.,1.));
#12792=DIRECTION('ref_axis',(1.,0.,0.));
#12793=DIRECTION('center_axis',(0.,0.,1.));
#12794=DIRECTION('ref_axis',(1.,0.,0.));
#12795=DIRECTION('',(0.,0.,-1.));
#12796=DIRECTION('center_axis',(0.,0.,1.));
#12797=DIRECTION('ref_axis',(1.,0.,0.));
#12798=DIRECTION('center_axis',(0.,0.,1.));
#12799=DIRECTION('ref_axis',(1.,0.,0.));
#12800=DIRECTION('axis',(0.,0.,1.));
#12801=DIRECTION('refdir',(1.,0.,0.));
#12802=DIRECTION('center_axis',(0.,0.,1.));
#12803=DIRECTION('ref_axis',(1.,0.,0.));
#12804=DIRECTION('center_axis',(0.,0.,-1.));
#12805=DIRECTION('ref_axis',(1.,0.,0.));
#12806=DIRECTION('',(0.,0.,-1.));
#12807=DIRECTION('center_axis',(0.,0.,-1.));
#12808=DIRECTION('ref_axis',(1.,0.,0.));
#12809=DIRECTION('center_axis',(0.,0.,1.));
#12810=DIRECTION('ref_axis',(1.,0.,0.));
#12811=DIRECTION('center_axis',(0.,0.,1.));
#12812=DIRECTION('ref_axis',(1.,0.,0.));
#12813=DIRECTION('',(0.,0.,-1.));
#12814=DIRECTION('center_axis',(0.,0.,1.));
#12815=DIRECTION('ref_axis',(1.,0.,0.));
#12816=DIRECTION('center_axis',(0.,0.,1.));
#12817=DIRECTION('ref_axis',(1.,0.,0.));
#12818=DIRECTION('center_axis',(0.,0.,1.));
#12819=DIRECTION('ref_axis',(1.,0.,0.));
#12820=DIRECTION('axis',(0.,0.,1.));
#12821=DIRECTION('refdir',(1.,0.,0.));
#12822=DIRECTION('center_axis',(0.,0.,1.));
#12823=DIRECTION('ref_axis',(1.,0.,0.));
#12824=DIRECTION('center_axis',(0.,0.,-1.));
#12825=DIRECTION('ref_axis',(1.,0.,0.));
#12826=DIRECTION('',(0.,0.,-1.));
#12827=DIRECTION('center_axis',(0.,0.,-1.));
#12828=DIRECTION('ref_axis',(1.,0.,0.));
#12829=DIRECTION('center_axis',(0.,0.,1.));
#12830=DIRECTION('ref_axis',(1.,0.,0.));
#12831=DIRECTION('center_axis',(0.,0.,1.));
#12832=DIRECTION('ref_axis',(1.,0.,0.));
#12833=DIRECTION('',(0.,0.,-1.));
#12834=DIRECTION('center_axis',(0.,0.,1.));
#12835=DIRECTION('ref_axis',(1.,0.,0.));
#12836=DIRECTION('center_axis',(0.,0.,1.));
#12837=DIRECTION('ref_axis',(1.,0.,0.));
#12838=DIRECTION('center_axis',(0.,0.,1.));
#12839=DIRECTION('ref_axis',(1.,0.,0.));
#12840=DIRECTION('axis',(0.,0.,1.));
#12841=DIRECTION('refdir',(1.,0.,0.));
#12842=DIRECTION('center_axis',(0.,0.,1.));
#12843=DIRECTION('ref_axis',(1.,0.,0.));
#12844=DIRECTION('center_axis',(0.,0.,-1.));
#12845=DIRECTION('ref_axis',(1.,0.,0.));
#12846=DIRECTION('',(0.,0.,-1.));
#12847=DIRECTION('center_axis',(0.,0.,-1.));
#12848=DIRECTION('ref_axis',(1.,0.,0.));
#12849=DIRECTION('center_axis',(0.,0.,1.));
#12850=DIRECTION('ref_axis',(1.,0.,0.));
#12851=DIRECTION('center_axis',(0.,0.,1.));
#12852=DIRECTION('ref_axis',(1.,0.,0.));
#12853=DIRECTION('',(0.,0.,-1.));
#12854=DIRECTION('center_axis',(0.,0.,1.));
#12855=DIRECTION('ref_axis',(1.,0.,0.));
#12856=DIRECTION('center_axis',(0.,0.,1.));
#12857=DIRECTION('ref_axis',(1.,0.,0.));
#12858=DIRECTION('center_axis',(0.,0.,1.));
#12859=DIRECTION('ref_axis',(1.,0.,0.));
#12860=DIRECTION('axis',(0.,0.,1.));
#12861=DIRECTION('refdir',(1.,0.,0.));
#12862=DIRECTION('axis',(0.,0.,1.));
#12863=DIRECTION('refdir',(1.,0.,0.));
#12864=DIRECTION('center_axis',(0.,0.,1.));
#12865=DIRECTION('ref_axis',(1.,0.,0.));
#12866=DIRECTION('center_axis',(0.,0.,1.));
#12867=DIRECTION('ref_axis',(1.,0.,0.));
#12868=DIRECTION('',(0.,0.,1.));
#12869=DIRECTION('center_axis',(0.,0.,-1.));
#12870=DIRECTION('ref_axis',(1.,0.,0.));
#12871=DIRECTION('center_axis',(0.,0.,1.));
#12872=DIRECTION('ref_axis',(1.,0.,0.));
#12873=DIRECTION('center_axis',(0.,1.,0.));
#12874=DIRECTION('ref_axis',(1.,0.,0.));
#12875=DIRECTION('center_axis',(0.,1.,0.));
#12876=DIRECTION('ref_axis',(1.,0.,0.));
#12877=DIRECTION('',(0.,1.,0.));
#12878=DIRECTION('center_axis',(0.,-1.,0.));
#12879=DIRECTION('ref_axis',(1.,0.,0.));
#12880=DIRECTION('center_axis',(0.,1.,0.));
#12881=DIRECTION('ref_axis',(1.,0.,0.));
#12882=DIRECTION('center_axis',(0.,1.,0.));
#12883=DIRECTION('ref_axis',(1.,0.,0.));
#12884=DIRECTION('',(0.,1.,0.));
#12885=DIRECTION('center_axis',(0.,-1.,0.));
#12886=DIRECTION('ref_axis',(1.,0.,0.));
#12887=DIRECTION('center_axis',(0.,1.,0.));
#12888=DIRECTION('ref_axis',(1.,0.,0.));
#12889=DIRECTION('center_axis',(0.,1.,0.));
#12890=DIRECTION('ref_axis',(1.,0.,0.));
#12891=DIRECTION('',(0.,1.,0.));
#12892=DIRECTION('center_axis',(0.,-1.,0.));
#12893=DIRECTION('ref_axis',(1.,0.,0.));
#12894=DIRECTION('center_axis',(0.,1.,0.));
#12895=DIRECTION('ref_axis',(1.,0.,0.));
#12896=DIRECTION('center_axis',(0.,1.,0.));
#12897=DIRECTION('ref_axis',(1.,0.,0.));
#12898=DIRECTION('',(0.,1.,0.));
#12899=DIRECTION('center_axis',(0.,-1.,0.));
#12900=DIRECTION('ref_axis',(1.,0.,0.));
#12901=DIRECTION('center_axis',(0.,1.,0.));
#12902=DIRECTION('ref_axis',(1.,0.,0.));
#12903=DIRECTION('center_axis',(0.,1.,0.));
#12904=DIRECTION('ref_axis',(1.,0.,0.));
#12905=DIRECTION('',(0.,1.,0.));
#12906=DIRECTION('center_axis',(0.,-1.,0.));
#12907=DIRECTION('ref_axis',(1.,0.,0.));
#12908=DIRECTION('center_axis',(0.,1.,0.));
#12909=DIRECTION('ref_axis',(-1.,0.,0.));
#12910=DIRECTION('',(-1.,0.,0.));
#12911=DIRECTION('',(0.,0.,1.));
#12912=DIRECTION('',(-1.,0.,0.));
#12913=DIRECTION('',(0.,0.,1.));
#12914=DIRECTION('center_axis',(1.,0.,0.));
#12915=DIRECTION('ref_axis',(0.,1.,0.));
#12916=DIRECTION('',(0.,1.,0.));
#12917=DIRECTION('',(0.,1.,0.));
#12918=DIRECTION('',(0.,0.,1.));
#12919=DIRECTION('center_axis',(0.,-1.,0.));
#12920=DIRECTION('ref_axis',(1.,0.,0.));
#12921=DIRECTION('',(1.,0.,0.));
#12922=DIRECTION('',(1.,0.,0.));
#12923=DIRECTION('',(0.,0.,1.));
#12924=DIRECTION('center_axis',(-1.,0.,0.));
#12925=DIRECTION('ref_axis',(0.,-1.,0.));
#12926=DIRECTION('',(0.,-1.,0.));
#12927=DIRECTION('',(0.,-1.,0.));
#12928=DIRECTION('center_axis',(0.,0.,1.));
#12929=DIRECTION('ref_axis',(1.,0.,0.));
#12930=DIRECTION('center_axis',(0.,0.,1.));
#12931=DIRECTION('ref_axis',(1.,0.,0.));
#12932=DIRECTION('axis',(0.,0.,1.));
#12933=DIRECTION('refdir',(1.,0.,0.));
#12934=DIRECTION('center_axis',(0.,1.,0.));
#12935=DIRECTION('ref_axis',(1.,0.,0.));
#12936=DIRECTION('center_axis',(0.,1.,0.));
#12937=DIRECTION('ref_axis',(1.,0.,0.));
#12938=DIRECTION('',(0.,1.,0.));
#12939=DIRECTION('center_axis',(0.,-1.,0.));
#12940=DIRECTION('ref_axis',(1.,0.,0.));
#12941=DIRECTION('center_axis',(0.,1.,0.));
#12942=DIRECTION('ref_axis',(1.,0.,0.));
#12943=DIRECTION('center_axis',(0.,1.,0.));
#12944=DIRECTION('ref_axis',(1.,0.,0.));
#12945=DIRECTION('',(0.,1.,0.));
#12946=DIRECTION('center_axis',(0.,-1.,0.));
#12947=DIRECTION('ref_axis',(1.,0.,0.));
#12948=DIRECTION('center_axis',(0.,1.,0.));
#12949=DIRECTION('ref_axis',(1.,0.,0.));
#12950=DIRECTION('center_axis',(0.,1.,0.));
#12951=DIRECTION('ref_axis',(1.,0.,0.));
#12952=DIRECTION('',(0.,1.,0.));
#12953=DIRECTION('center_axis',(0.,-1.,0.));
#12954=DIRECTION('ref_axis',(1.,0.,0.));
#12955=DIRECTION('center_axis',(0.,1.,0.));
#12956=DIRECTION('ref_axis',(1.,0.,0.));
#12957=DIRECTION('center_axis',(0.,1.,0.));
#12958=DIRECTION('ref_axis',(1.,0.,0.));
#12959=DIRECTION('',(0.,1.,0.));
#12960=DIRECTION('center_axis',(0.,-1.,0.));
#12961=DIRECTION('ref_axis',(1.,0.,0.));
#12962=DIRECTION('center_axis',(0.,1.,0.));
#12963=DIRECTION('ref_axis',(1.,0.,0.));
#12964=DIRECTION('center_axis',(0.,1.,0.));
#12965=DIRECTION('ref_axis',(1.,0.,0.));
#12966=DIRECTION('',(0.,1.,0.));
#12967=DIRECTION('center_axis',(0.,-1.,0.));
#12968=DIRECTION('ref_axis',(1.,0.,0.));
#12969=DIRECTION('center_axis',(0.,1.,0.));
#12970=DIRECTION('ref_axis',(-1.,0.,0.));
#12971=DIRECTION('',(-1.,0.,0.));
#12972=DIRECTION('',(0.,0.,1.));
#12973=DIRECTION('',(-1.,0.,0.));
#12974=DIRECTION('',(0.,0.,1.));
#12975=DIRECTION('center_axis',(1.,0.,0.));
#12976=DIRECTION('ref_axis',(0.,1.,0.));
#12977=DIRECTION('',(0.,1.,0.));
#12978=DIRECTION('',(0.,1.,0.));
#12979=DIRECTION('',(0.,0.,1.));
#12980=DIRECTION('center_axis',(0.,-1.,0.));
#12981=DIRECTION('ref_axis',(1.,0.,0.));
#12982=DIRECTION('',(1.,0.,0.));
#12983=DIRECTION('',(1.,0.,0.));
#12984=DIRECTION('',(0.,0.,1.));
#12985=DIRECTION('center_axis',(-1.,0.,0.));
#12986=DIRECTION('ref_axis',(0.,-1.,0.));
#12987=DIRECTION('',(0.,-1.,0.));
#12988=DIRECTION('',(0.,-1.,0.));
#12989=DIRECTION('center_axis',(0.,0.,1.));
#12990=DIRECTION('ref_axis',(1.,0.,0.));
#12991=DIRECTION('center_axis',(0.,0.,1.));
#12992=DIRECTION('ref_axis',(1.,0.,0.));
#12993=DIRECTION('axis',(0.,0.,1.));
#12994=DIRECTION('refdir',(1.,0.,0.));
#12995=DIRECTION('center_axis',(0.,1.,0.));
#12996=DIRECTION('ref_axis',(1.,0.,0.));
#12997=DIRECTION('center_axis',(0.,1.,0.));
#12998=DIRECTION('ref_axis',(1.,0.,0.));
#12999=DIRECTION('',(0.,1.,0.));
#13000=DIRECTION('center_axis',(0.,-1.,0.));
#13001=DIRECTION('ref_axis',(1.,0.,0.));
#13002=DIRECTION('center_axis',(0.,1.,0.));
#13003=DIRECTION('ref_axis',(1.,0.,0.));
#13004=DIRECTION('center_axis',(0.,1.,0.));
#13005=DIRECTION('ref_axis',(1.,0.,0.));
#13006=DIRECTION('',(0.,1.,0.));
#13007=DIRECTION('center_axis',(0.,-1.,0.));
#13008=DIRECTION('ref_axis',(1.,0.,0.));
#13009=DIRECTION('center_axis',(0.,1.,0.));
#13010=DIRECTION('ref_axis',(1.,0.,0.));
#13011=DIRECTION('center_axis',(0.,1.,0.));
#13012=DIRECTION('ref_axis',(1.,0.,0.));
#13013=DIRECTION('',(0.,1.,0.));
#13014=DIRECTION('center_axis',(0.,-1.,0.));
#13015=DIRECTION('ref_axis',(1.,0.,0.));
#13016=DIRECTION('center_axis',(0.,1.,0.));
#13017=DIRECTION('ref_axis',(1.,0.,0.));
#13018=DIRECTION('center_axis',(0.,1.,0.));
#13019=DIRECTION('ref_axis',(1.,0.,0.));
#13020=DIRECTION('',(0.,1.,0.));
#13021=DIRECTION('center_axis',(0.,-1.,0.));
#13022=DIRECTION('ref_axis',(1.,0.,0.));
#13023=DIRECTION('center_axis',(0.,1.,0.));
#13024=DIRECTION('ref_axis',(1.,0.,0.));
#13025=DIRECTION('center_axis',(0.,1.,0.));
#13026=DIRECTION('ref_axis',(1.,0.,0.));
#13027=DIRECTION('',(0.,1.,0.));
#13028=DIRECTION('center_axis',(0.,-1.,0.));
#13029=DIRECTION('ref_axis',(1.,0.,0.));
#13030=DIRECTION('center_axis',(0.,1.,0.));
#13031=DIRECTION('ref_axis',(-1.,0.,0.));
#13032=DIRECTION('',(-1.,0.,0.));
#13033=DIRECTION('',(0.,0.,1.));
#13034=DIRECTION('',(-1.,0.,0.));
#13035=DIRECTION('',(0.,0.,1.));
#13036=DIRECTION('center_axis',(1.,0.,0.));
#13037=DIRECTION('ref_axis',(0.,1.,0.));
#13038=DIRECTION('',(0.,1.,0.));
#13039=DIRECTION('',(0.,1.,0.));
#13040=DIRECTION('',(0.,0.,1.));
#13041=DIRECTION('center_axis',(0.,-1.,0.));
#13042=DIRECTION('ref_axis',(1.,0.,0.));
#13043=DIRECTION('',(1.,0.,0.));
#13044=DIRECTION('',(1.,0.,0.));
#13045=DIRECTION('',(0.,0.,1.));
#13046=DIRECTION('center_axis',(-1.,0.,0.));
#13047=DIRECTION('ref_axis',(0.,-1.,0.));
#13048=DIRECTION('',(0.,-1.,0.));
#13049=DIRECTION('',(0.,-1.,0.));
#13050=DIRECTION('center_axis',(0.,0.,1.));
#13051=DIRECTION('ref_axis',(1.,0.,0.));
#13052=DIRECTION('center_axis',(0.,0.,1.));
#13053=DIRECTION('ref_axis',(1.,0.,0.));
#13054=DIRECTION('axis',(0.,0.,1.));
#13055=DIRECTION('refdir',(1.,0.,0.));
#13056=DIRECTION('center_axis',(0.,0.,1.));
#13057=DIRECTION('ref_axis',(1.,0.,0.));
#13058=DIRECTION('center_axis',(0.,0.,1.));
#13059=DIRECTION('ref_axis',(1.,0.,0.));
#13060=DIRECTION('',(0.,0.,1.));
#13061=DIRECTION('center_axis',(0.,0.,-1.));
#13062=DIRECTION('ref_axis',(1.,0.,0.));
#13063=DIRECTION('center_axis',(0.,0.,1.));
#13064=DIRECTION('ref_axis',(1.,0.,0.));
#13065=DIRECTION('center_axis',(0.,0.,1.));
#13066=DIRECTION('ref_axis',(1.,0.,0.));
#13067=DIRECTION('center_axis',(0.,0.,1.));
#13068=DIRECTION('ref_axis',(1.,0.,0.));
#13069=DIRECTION('center_axis',(0.,0.,1.));
#13070=DIRECTION('ref_axis',(1.,0.,0.));
#13071=DIRECTION('center_axis',(0.,0.,1.));
#13072=DIRECTION('ref_axis',(1.,0.,0.));
#13073=DIRECTION('center_axis',(0.,0.,1.));
#13074=DIRECTION('ref_axis',(1.,0.,0.));
#13075=DIRECTION('center_axis',(0.,0.,-1.));
#13076=DIRECTION('ref_axis',(1.,0.,0.));
#13077=DIRECTION('center_axis',(0.,0.,1.));
#13078=DIRECTION('ref_axis',(1.,0.,0.));
#13079=DIRECTION('',(0.,0.,-1.));
#13080=DIRECTION('center_axis',(0.,0.,1.));
#13081=DIRECTION('ref_axis',(1.,0.,0.));
#13082=DIRECTION('',(0.,0.,-1.));
#13083=DIRECTION('center_axis',(0.,0.,1.));
#13084=DIRECTION('ref_axis',(1.,0.,0.));
#13085=DIRECTION('center_axis',(0.,0.,1.));
#13086=DIRECTION('ref_axis',(1.,0.,0.));
#13087=DIRECTION('center_axis',(0.,0.,1.));
#13088=DIRECTION('ref_axis',(1.,0.,0.));
#13089=DIRECTION('',(0.,0.,-1.));
#13090=DIRECTION('center_axis',(0.,0.,1.));
#13091=DIRECTION('ref_axis',(1.,0.,0.));
#13092=DIRECTION('center_axis',(0.,0.,1.));
#13093=DIRECTION('ref_axis',(1.,0.,0.));
#13094=DIRECTION('axis',(0.,0.,1.));
#13095=DIRECTION('refdir',(1.,0.,0.));
#13096=DIRECTION('center_axis',(0.,0.,1.));
#13097=DIRECTION('ref_axis',(1.,0.,0.));
#13098=DIRECTION('center_axis',(0.,0.,-1.));
#13099=DIRECTION('ref_axis',(1.,0.,0.));
#13100=DIRECTION('',(0.,0.,-1.));
#13101=DIRECTION('center_axis',(0.,0.,-1.));
#13102=DIRECTION('ref_axis',(1.,0.,0.));
#13103=DIRECTION('center_axis',(0.,0.,1.));
#13104=DIRECTION('ref_axis',(1.,0.,0.));
#13105=DIRECTION('center_axis',(0.,0.,1.));
#13106=DIRECTION('ref_axis',(1.,0.,0.));
#13107=DIRECTION('',(0.,0.,-1.));
#13108=DIRECTION('center_axis',(0.,0.,1.));
#13109=DIRECTION('ref_axis',(1.,0.,0.));
#13110=DIRECTION('center_axis',(0.,0.,1.));
#13111=DIRECTION('ref_axis',(1.,0.,0.));
#13112=DIRECTION('center_axis',(0.,0.,1.));
#13113=DIRECTION('ref_axis',(1.,0.,0.));
#13114=DIRECTION('axis',(0.,0.,1.));
#13115=DIRECTION('refdir',(1.,0.,0.));
#13116=DIRECTION('center_axis',(0.,0.,1.));
#13117=DIRECTION('ref_axis',(1.,0.,0.));
#13118=DIRECTION('center_axis',(0.,0.,-1.));
#13119=DIRECTION('ref_axis',(1.,0.,0.));
#13120=DIRECTION('',(0.,0.,-1.));
#13121=DIRECTION('center_axis',(0.,0.,-1.));
#13122=DIRECTION('ref_axis',(1.,0.,0.));
#13123=DIRECTION('center_axis',(0.,0.,1.));
#13124=DIRECTION('ref_axis',(1.,0.,0.));
#13125=DIRECTION('center_axis',(0.,0.,1.));
#13126=DIRECTION('ref_axis',(1.,0.,0.));
#13127=DIRECTION('',(0.,0.,-1.));
#13128=DIRECTION('center_axis',(0.,0.,1.));
#13129=DIRECTION('ref_axis',(1.,0.,0.));
#13130=DIRECTION('center_axis',(0.,0.,1.));
#13131=DIRECTION('ref_axis',(1.,0.,0.));
#13132=DIRECTION('center_axis',(0.,0.,1.));
#13133=DIRECTION('ref_axis',(1.,0.,0.));
#13134=DIRECTION('axis',(0.,0.,1.));
#13135=DIRECTION('refdir',(1.,0.,0.));
#13136=DIRECTION('center_axis',(0.,0.,1.));
#13137=DIRECTION('ref_axis',(1.,0.,0.));
#13138=DIRECTION('center_axis',(0.,0.,-1.));
#13139=DIRECTION('ref_axis',(1.,0.,0.));
#13140=DIRECTION('',(0.,0.,-1.));
#13141=DIRECTION('center_axis',(0.,0.,-1.));
#13142=DIRECTION('ref_axis',(1.,0.,0.));
#13143=DIRECTION('center_axis',(0.,0.,1.));
#13144=DIRECTION('ref_axis',(1.,0.,0.));
#13145=DIRECTION('center_axis',(0.,0.,1.));
#13146=DIRECTION('ref_axis',(1.,0.,0.));
#13147=DIRECTION('',(0.,0.,-1.));
#13148=DIRECTION('center_axis',(0.,0.,1.));
#13149=DIRECTION('ref_axis',(1.,0.,0.));
#13150=DIRECTION('center_axis',(0.,0.,1.));
#13151=DIRECTION('ref_axis',(1.,0.,0.));
#13152=DIRECTION('center_axis',(0.,0.,1.));
#13153=DIRECTION('ref_axis',(1.,0.,0.));
#13154=DIRECTION('axis',(0.,0.,1.));
#13155=DIRECTION('refdir',(1.,0.,0.));
#13156=DIRECTION('axis',(0.,0.,1.));
#13157=DIRECTION('refdir',(1.,0.,0.));
#13158=DIRECTION('center_axis',(0.,1.,0.));
#13159=DIRECTION('ref_axis',(0.,0.,1.));
#13160=DIRECTION('center_axis',(0.,-1.,0.));
#13161=DIRECTION('ref_axis',(1.,0.,0.));
#13162=DIRECTION('',(-1.,0.,0.));
#13163=DIRECTION('',(0.,0.,-1.));
#13164=DIRECTION('',(1.,0.,0.));
#13165=DIRECTION('center_axis',(0.,0.,1.));
#13166=DIRECTION('ref_axis',(1.,0.,0.));
#13167=DIRECTION('',(0.,-1.,0.));
#13168=DIRECTION('',(0.,1.,0.));
#13169=DIRECTION('',(-1.,0.,0.));
#13170=DIRECTION('center_axis',(0.,-1.,0.));
#13171=DIRECTION('ref_axis',(0.,0.,-1.));
#13172=DIRECTION('center_axis',(0.,1.,0.));
#13173=DIRECTION('ref_axis',(1.,0.,0.));
#13174=DIRECTION('',(0.,0.,1.));
#13175=DIRECTION('',(1.,0.,0.));
#13176=DIRECTION('center_axis',(0.,0.,-1.));
#13177=DIRECTION('ref_axis',(-1.,0.,0.));
#13178=DIRECTION('',(0.,1.,0.));
#13179=DIRECTION('',(0.,1.,0.));
#13180=DIRECTION('center_axis',(1.,0.,0.));
#13181=DIRECTION('ref_axis',(0.,0.,-1.));
#13182=DIRECTION('center_axis',(0.,1.,0.));
#13183=DIRECTION('ref_axis',(0.,0.,1.));
#13184=DIRECTION('center_axis',(0.,-1.,0.));
#13185=DIRECTION('ref_axis',(1.,0.,0.));
#13186=DIRECTION('center_axis',(0.,-1.,0.));
#13187=DIRECTION('ref_axis',(1.,0.,0.));
#13188=DIRECTION('center_axis',(0.,-1.,0.));
#13189=DIRECTION('ref_axis',(1.,0.,0.));
#13190=DIRECTION('center_axis',(0.,-1.,0.));
#13191=DIRECTION('ref_axis',(1.,0.,0.));
#13192=DIRECTION('',(0.,1.,0.));
#13193=DIRECTION('center_axis',(0.,-1.,0.));
#13194=DIRECTION('ref_axis',(0.,0.,-1.));
#13195=DIRECTION('center_axis',(0.,-1.,0.));
#13196=DIRECTION('ref_axis',(1.,0.,0.));
#13197=DIRECTION('center_axis',(0.,-1.,0.));
#13198=DIRECTION('ref_axis',(1.,0.,0.));
#13199=DIRECTION('center_axis',(0.,-1.,0.));
#13200=DIRECTION('ref_axis',(1.,0.,0.));
#13201=DIRECTION('',(0.,1.,0.));
#13202=DIRECTION('center_axis',(0.,1.,0.));
#13203=DIRECTION('ref_axis',(0.,0.,1.));
#13204=DIRECTION('center_axis',(0.,-1.,0.));
#13205=DIRECTION('ref_axis',(1.,0.,0.));
#13206=DIRECTION('center_axis',(0.,-1.,0.));
#13207=DIRECTION('ref_axis',(1.,0.,0.));
#13208=DIRECTION('center_axis',(0.,-1.,0.));
#13209=DIRECTION('ref_axis',(1.,0.,0.));
#13210=DIRECTION('',(0.,1.,0.));
#13211=DIRECTION('center_axis',(0.,-1.,0.));
#13212=DIRECTION('ref_axis',(0.,0.,-1.));
#13213=DIRECTION('center_axis',(0.,-1.,0.));
#13214=DIRECTION('ref_axis',(1.,0.,0.));
#13215=DIRECTION('center_axis',(0.,-1.,0.));
#13216=DIRECTION('ref_axis',(1.,0.,0.));
#13217=DIRECTION('center_axis',(0.,-1.,0.));
#13218=DIRECTION('ref_axis',(1.,0.,0.));
#13219=DIRECTION('',(0.,1.,0.));
#13220=DIRECTION('center_axis',(0.,1.,0.));
#13221=DIRECTION('ref_axis',(0.,0.,1.));
#13222=DIRECTION('center_axis',(0.,-1.,0.));
#13223=DIRECTION('ref_axis',(1.,0.,0.));
#13224=DIRECTION('center_axis',(0.,-1.,0.));
#13225=DIRECTION('ref_axis',(1.,0.,0.));
#13226=DIRECTION('center_axis',(0.,-1.,0.));
#13227=DIRECTION('ref_axis',(1.,0.,0.));
#13228=DIRECTION('',(0.,1.,0.));
#13229=DIRECTION('center_axis',(0.,-1.,0.));
#13230=DIRECTION('ref_axis',(0.,0.,-1.));
#13231=DIRECTION('center_axis',(0.,-1.,0.));
#13232=DIRECTION('ref_axis',(1.,0.,0.));
#13233=DIRECTION('center_axis',(0.,-1.,0.));
#13234=DIRECTION('ref_axis',(1.,0.,0.));
#13235=DIRECTION('',(0.,1.,0.));
#13236=DIRECTION('axis',(0.,0.,1.));
#13237=DIRECTION('refdir',(1.,0.,0.));
#13238=DIRECTION('center_axis',(0.,1.,0.));
#13239=DIRECTION('ref_axis',(0.,0.,1.));
#13240=DIRECTION('center_axis',(0.,1.,0.));
#13241=DIRECTION('ref_axis',(1.,0.,0.));
#13242=DIRECTION('',(1.,0.,0.));
#13243=DIRECTION('center_axis',(0.,-1.,0.));
#13244=DIRECTION('ref_axis',(1.,0.,0.));
#13245=DIRECTION('',(-1.,0.,0.));
#13246=DIRECTION('center_axis',(0.,0.,-1.));
#13247=DIRECTION('ref_axis',(-1.,0.,0.));
#13248=DIRECTION('',(0.,-1.,0.));
#13249=DIRECTION('',(0.,1.,0.));
#13250=DIRECTION('',(1.,0.,0.));
#13251=DIRECTION('center_axis',(0.,-1.,0.));
#13252=DIRECTION('ref_axis',(0.,0.,-1.));
#13253=DIRECTION('center_axis',(0.,-1.,0.));
#13254=DIRECTION('ref_axis',(1.,0.,0.));
#13255=DIRECTION('center_axis',(0.,1.,0.));
#13256=DIRECTION('ref_axis',(1.,0.,0.));
#13257=DIRECTION('',(-1.,0.,0.));
#13258=DIRECTION('center_axis',(0.,0.,1.));
#13259=DIRECTION('ref_axis',(1.,0.,0.));
#13260=DIRECTION('',(0.,1.,0.));
#13261=DIRECTION('',(0.,-1.,0.));
#13262=DIRECTION('center_axis',(0.,1.,0.));
#13263=DIRECTION('ref_axis',(0.,0.,1.));
#13264=DIRECTION('center_axis',(0.,-1.,0.));
#13265=DIRECTION('ref_axis',(1.,0.,0.));
#13266=DIRECTION('center_axis',(0.,-1.,0.));
#13267=DIRECTION('ref_axis',(1.,0.,0.));
#13268=DIRECTION('center_axis',(0.,-1.,0.));
#13269=DIRECTION('ref_axis',(1.,0.,0.));
#13270=DIRECTION('center_axis',(0.,-1.,0.));
#13271=DIRECTION('ref_axis',(1.,0.,0.));
#13272=DIRECTION('',(0.,1.,0.));
#13273=DIRECTION('center_axis',(0.,-1.,0.));
#13274=DIRECTION('ref_axis',(0.,0.,-1.));
#13275=DIRECTION('center_axis',(0.,-1.,0.));
#13276=DIRECTION('ref_axis',(1.,0.,0.));
#13277=DIRECTION('center_axis',(0.,-1.,0.));
#13278=DIRECTION('ref_axis',(1.,0.,0.));
#13279=DIRECTION('',(0.,1.,0.));
#13280=DIRECTION('',(0.,0.,1.));
#13281=DIRECTION('',(1.,0.,0.));
#13282=DIRECTION('',(0.,0.,1.));
#13283=DIRECTION('',(1.,0.,0.));
#13284=DIRECTION('axis',(0.,0.,1.));
#13285=DIRECTION('refdir',(1.,0.,0.));
#13286=DIRECTION('center_axis',(0.866025403784439,0.,-0.5));
#13287=DIRECTION('ref_axis',(0.5,0.,0.866025403784439));
#13288=DIRECTION('',(-0.5,0.,-0.866025403784439));
#13289=DIRECTION('',(0.,-1.,0.));
#13290=DIRECTION('',(0.5,0.,0.866025403784439));
#13291=DIRECTION('',(0.,-1.,0.));
#13292=DIRECTION('center_axis',(1.60246890531964E-16,0.,-1.));
#13293=DIRECTION('ref_axis',(1.,0.,1.60246890531964E-16));
#13294=DIRECTION('',(-1.,0.,-1.60246890531964E-16));
#13295=DIRECTION('',(0.,-1.,0.));
#13296=DIRECTION('',(1.,0.,1.60246890531964E-16));
#13297=DIRECTION('center_axis',(-0.866025403784439,0.,-0.5));
#13298=DIRECTION('ref_axis',(0.5,0.,-0.866025403784439));
#13299=DIRECTION('',(-0.5,0.,0.866025403784439));
#13300=DIRECTION('',(0.,-1.,0.));
#13301=DIRECTION('',(0.5,0.,-0.866025403784439));
#13302=DIRECTION('center_axis',(-0.866025403784439,0.,0.5));
#13303=DIRECTION('ref_axis',(-0.5,0.,-0.866025403784439));
#13304=DIRECTION('',(0.5,0.,0.866025403784439));
#13305=DIRECTION('',(0.,-1.,0.));
#13306=DIRECTION('',(-0.5,0.,-0.866025403784439));
#13307=DIRECTION('center_axis',(-1.60246890531964E-16,0.,1.));
#13308=DIRECTION('ref_axis',(-1.,0.,-1.60246890531964E-16));
#13309=DIRECTION('',(1.,0.,1.60246890531964E-16));
#13310=DIRECTION('',(0.,-1.,0.));
#13311=DIRECTION('',(-1.,0.,-1.60246890531964E-16));
#13312=DIRECTION('center_axis',(0.866025403784439,0.,0.5));
#13313=DIRECTION('ref_axis',(-0.5,0.,0.866025403784439));
#13314=DIRECTION('',(0.5,0.,-0.866025403784439));
#13315=DIRECTION('',(-0.5,0.,0.866025403784439));
#13316=DIRECTION('center_axis',(0.,1.,0.));
#13317=DIRECTION('ref_axis',(1.,0.,0.));
#13318=DIRECTION('center_axis',(0.,-1.,0.));
#13319=DIRECTION('ref_axis',(0.,0.,-1.));
#13320=DIRECTION('center_axis',(0.,1.,0.));
#13321=DIRECTION('ref_axis',(1.,0.,0.));
#13322=DIRECTION('center_axis',(0.,1.,0.));
#13323=DIRECTION('ref_axis',(1.,0.,0.));
#13324=DIRECTION('center_axis',(0.,1.,0.));
#13325=DIRECTION('ref_axis',(0.,0.,1.));
#13326=DIRECTION('center_axis',(0.,-1.,0.));
#13327=DIRECTION('ref_axis',(1.,0.,0.));
#13328=DIRECTION('center_axis',(0.,-1.,0.));
#13329=DIRECTION('ref_axis',(1.,0.,0.));
#13330=DIRECTION('center_axis',(0.,-1.,0.));
#13331=DIRECTION('ref_axis',(1.,0.,0.));
#13332=DIRECTION('',(0.707106781186547,0.707106781186548,8.65956056235493E-17));
#13333=DIRECTION('center_axis',(0.,-1.,0.));
#13334=DIRECTION('ref_axis',(1.,0.,0.));
#13335=DIRECTION('center_axis',(0.,-1.,0.));
#13336=DIRECTION('ref_axis',(1.,0.,0.));
#13337=DIRECTION('',(0.,1.,0.));
#13338=DIRECTION('center_axis',(0.,1.,0.));
#13339=DIRECTION('ref_axis',(1.,0.,0.));
#13340=DIRECTION('center_axis',(0.,-1.,0.));
#13341=DIRECTION('ref_axis',(1.,0.,0.));
#13342=DIRECTION('',(-0.707106781186547,0.707106781186548,-8.65956056235493E-17));
#13343=DIRECTION('center_axis',(0.,-1.,0.));
#13344=DIRECTION('ref_axis',(0.,0.,-1.));
#13345=DIRECTION('center_axis',(0.,-1.,0.));
#13346=DIRECTION('ref_axis',(1.,0.,0.));
#13347=DIRECTION('center_axis',(0.,1.,0.));
#13348=DIRECTION('ref_axis',(1.,0.,0.));
#13349=DIRECTION('center_axis',(0.,1.,0.));
#13350=DIRECTION('ref_axis',(1.,0.,0.));
#13351=DIRECTION('',(-0.447213595499958,0.894427190999916,-5.47678698264203E-17));
#13352=DIRECTION('center_axis',(0.,-1.,0.));
#13353=DIRECTION('ref_axis',(1.,0.,0.));
#13354=DIRECTION('',(0.,1.,0.));
#13355=DIRECTION('',(0.,0.,1.));
#13356=DIRECTION('',(1.,0.,0.));
#13357=DIRECTION('',(0.,0.,1.));
#13358=DIRECTION('',(1.,0.,0.));
#13359=DIRECTION('',(0.,0.,1.));
#13360=DIRECTION('',(1.,0.,0.));
#13361=DIRECTION('',(0.,0.,1.));
#13362=DIRECTION('',(1.,0.,0.));
#13363=DIRECTION('',(0.,0.,1.));
#13364=DIRECTION('',(1.,0.,0.));
#13365=DIRECTION('',(0.,0.,1.));
#13366=DIRECTION('',(1.,0.,0.));
#13367=DIRECTION('',(0.,0.,1.));
#13368=DIRECTION('',(1.,0.,0.));
#13369=DIRECTION('',(0.,0.,1.));
#13370=DIRECTION('',(1.,0.,0.));
#13371=DIRECTION('',(0.,0.,1.));
#13372=DIRECTION('',(1.,0.,0.));
#13373=DIRECTION('',(0.,-1.,2.22044604925031E-16));
#13374=DIRECTION('',(1.,0.,0.));
#13375=DIRECTION('',(0.,-1.,2.22044604925031E-16));
#13376=DIRECTION('',(1.,0.,0.));
#13377=DIRECTION('',(0.,-1.,2.22044604925031E-16));
#13378=DIRECTION('',(1.,0.,0.));
#13379=DIRECTION('',(0.,-1.,2.22044604925031E-16));
#13380=DIRECTION('',(1.,0.,0.));
#13381=DIRECTION('',(0.,-1.,2.22044604925031E-16));
#13382=DIRECTION('',(1.,0.,0.));
#13383=DIRECTION('',(0.,-1.,2.22044604925031E-16));
#13384=DIRECTION('',(1.,0.,0.));
#13385=DIRECTION('',(0.,-1.,2.22044604925031E-16));
#13386=DIRECTION('',(1.,0.,0.));
#13387=DIRECTION('',(0.,-1.,2.22044604925031E-16));
#13388=DIRECTION('',(1.,0.,0.));
#13389=DIRECTION('',(0.,-1.,2.22044604925031E-16));
#13390=DIRECTION('',(1.,0.,0.));
#13391=DIRECTION('',(0.,0.,1.));
#13392=DIRECTION('',(1.,0.,0.));
#13393=DIRECTION('',(0.,-1.,2.22044604925031E-16));
#13394=DIRECTION('',(1.,0.,0.));
#13395=DIRECTION('',(0.,-1.,2.22044604925031E-16));
#13396=DIRECTION('',(1.,0.,0.));
#13397=DIRECTION('',(0.,-1.,2.22044604925031E-16));
#13398=DIRECTION('',(1.,0.,0.));
#13399=DIRECTION('',(0.,-1.,2.22044604925031E-16));
#13400=DIRECTION('',(1.,0.,0.));
#13401=DIRECTION('',(0.,-1.,2.22044604925031E-16));
#13402=DIRECTION('',(1.,0.,0.));
#13403=DIRECTION('',(0.,-1.,2.22044604925031E-16));
#13404=DIRECTION('',(1.,0.,0.));
#13405=DIRECTION('',(0.,0.,1.));
#13406=DIRECTION('',(2.22044604925031E-16,1.,0.));
#13407=DIRECTION('',(0.,-1.,2.22044604925031E-16));
#13408=DIRECTION('',(1.,0.,0.));
#13409=DIRECTION('',(0.,-1.,2.22044604925031E-16));
#13410=DIRECTION('',(1.,0.,0.));
#13411=DIRECTION('',(0.,-1.,2.22044604925031E-16));
#13412=DIRECTION('',(1.,0.,0.));
#13413=DIRECTION('',(0.,-1.,2.22044604925031E-16));
#13414=DIRECTION('',(1.,0.,0.));
#13415=DIRECTION('',(0.,-1.,2.22044604925031E-16));
#13416=DIRECTION('',(1.,0.,0.));
#13417=DIRECTION('',(0.,-1.,2.22044604925031E-16));
#13418=DIRECTION('',(1.,0.,0.));
#13419=DIRECTION('',(0.,0.,1.));
#13420=DIRECTION('',(1.,0.,0.));
#13421=DIRECTION('',(0.,0.,1.));
#13422=DIRECTION('',(1.,0.,0.));
#13423=DIRECTION('',(0.,0.,1.));
#13424=DIRECTION('',(1.,0.,0.));
#13425=DIRECTION('',(0.,0.,1.));
#13426=DIRECTION('',(1.,0.,0.));
#13427=DIRECTION('',(0.,0.,1.));
#13428=DIRECTION('',(1.,0.,0.));
#13429=DIRECTION('',(0.,0.,1.));
#13430=DIRECTION('',(1.,0.,0.));
#13431=DIRECTION('',(0.,0.,1.));
#13432=DIRECTION('',(1.,0.,0.));
#13433=DIRECTION('',(0.,0.,1.));
#13434=DIRECTION('',(1.,0.,0.));
#13435=DIRECTION('',(0.,0.,1.));
#13436=DIRECTION('',(1.,0.,0.));
#13437=DIRECTION('',(0.,0.,1.));
#13438=DIRECTION('',(1.,0.,0.));
#13439=DIRECTION('',(0.,0.,1.));
#13440=DIRECTION('',(1.,0.,0.));
#13441=DIRECTION('',(0.,0.,1.));
#13442=DIRECTION('',(1.,0.,0.));
#13443=DIRECTION('',(0.,1.,2.22044604925031E-16));
#13444=DIRECTION('',(1.,0.,0.));
#13445=DIRECTION('',(0.,0.,1.));
#13446=DIRECTION('',(2.22044604925031E-16,-1.,0.));
#13447=DIRECTION('',(0.,-1.,2.22044604925031E-16));
#13448=DIRECTION('',(1.,0.,0.));
#13449=DIRECTION('',(0.,-1.,2.22044604925031E-16));
#13450=DIRECTION('',(1.,0.,0.));
#13451=DIRECTION('',(0.,0.,1.));
#13452=DIRECTION('',(1.,0.,0.));
#13453=DIRECTION('',(0.,0.,1.));
#13454=DIRECTION('',(1.,0.,0.));
#13455=DIRECTION('',(0.,0.,1.));
#13456=DIRECTION('',(1.,0.,0.));
#13457=DIRECTION('',(0.,0.,1.));
#13458=DIRECTION('',(1.,0.,0.));
#13459=DIRECTION('',(0.,0.,1.));
#13460=DIRECTION('',(1.,0.,0.));
#13461=DIRECTION('',(0.,0.,1.));
#13462=DIRECTION('',(1.,0.,0.));
#13463=DIRECTION('',(0.,0.,1.));
#13464=DIRECTION('',(1.,0.,0.));
#13465=DIRECTION('',(0.,0.,1.));
#13466=DIRECTION('',(2.22044604925031E-16,-1.,0.));
#13467=DIRECTION('',(0.,0.,1.));
#13468=DIRECTION('',(2.22044604925031E-16,1.,0.));
#13469=DIRECTION('',(0.,0.,1.));
#13470=DIRECTION('',(2.22044604925031E-16,1.,0.));
#13471=DIRECTION('',(0.,0.,1.));
#13472=DIRECTION('',(2.22044604925031E-16,1.,0.));
#13473=DIRECTION('',(0.,0.,1.));
#13474=DIRECTION('',(2.22044604925031E-16,1.,0.));
#13475=DIRECTION('',(0.,0.,1.));
#13476=DIRECTION('',(2.22044604925031E-16,-1.,0.));
#13477=DIRECTION('',(0.,0.,1.));
#13478=DIRECTION('',(2.22044604925031E-16,-1.,0.));
#13479=DIRECTION('',(0.,0.,1.));
#13480=DIRECTION('',(2.22044604925031E-16,-1.,0.));
#13481=DIRECTION('',(0.,0.,1.));
#13482=DIRECTION('',(2.22044604925031E-16,-1.,0.));
#13483=DIRECTION('',(0.,-1.,2.22044604925031E-16));
#13484=DIRECTION('',(1.,0.,0.));
#13485=DIRECTION('',(0.,0.,1.));
#13486=DIRECTION('',(1.,0.,0.));
#13487=DIRECTION('',(0.,0.,1.));
#13488=DIRECTION('',(1.,0.,0.));
#13489=DIRECTION('',(0.,0.,1.));
#13490=DIRECTION('',(1.,0.,0.));
#13491=DIRECTION('',(0.,0.,1.));
#13492=DIRECTION('',(1.,0.,0.));
#13493=DIRECTION('',(0.,0.,1.));
#13494=DIRECTION('',(1.,0.,0.));
#13495=DIRECTION('',(0.,0.,1.));
#13496=DIRECTION('',(1.,0.,0.));
#13497=DIRECTION('',(0.,0.,1.));
#13498=DIRECTION('',(1.,0.,0.));
#13499=DIRECTION('',(0.,0.,1.));
#13500=DIRECTION('',(1.,0.,0.));
#13501=DIRECTION('',(0.,0.,1.));
#13502=DIRECTION('',(-1.,1.22464679914735E-16,0.));
#13503=DIRECTION('',(0.,0.,1.));
#13504=DIRECTION('',(-1.,1.22464679914735E-16,0.));
#13505=DIRECTION('',(0.,0.,1.));
#13506=DIRECTION('',(-1.,1.22464679914735E-16,0.));
#13507=DIRECTION('',(0.,0.,1.));
#13508=DIRECTION('',(-1.,1.22464679914735E-16,0.));
#13509=DIRECTION('',(0.,0.,1.));
#13510=DIRECTION('',(1.,0.,0.));
#13511=DIRECTION('',(0.,0.,1.));
#13512=DIRECTION('',(1.,0.,0.));
#13513=DIRECTION('',(0.,0.,1.));
#13514=DIRECTION('',(1.,0.,0.));
#13515=DIRECTION('',(0.,0.,1.));
#13516=DIRECTION('',(1.,0.,0.));
#13517=DIRECTION('',(0.,-1.,2.22044604925031E-16));
#13518=DIRECTION('',(1.,0.,0.));
#13519=DIRECTION('',(0.,0.,1.));
#13520=DIRECTION('',(1.,0.,0.));
#13521=DIRECTION('',(0.,0.,1.));
#13522=DIRECTION('',(1.,0.,0.));
#13523=DIRECTION('',(0.,0.,1.));
#13524=DIRECTION('',(1.,0.,0.));
#13525=DIRECTION('',(0.,0.,1.));
#13526=DIRECTION('',(1.,0.,0.));
#13527=DIRECTION('',(0.,0.,1.));
#13528=DIRECTION('',(1.,0.,0.));
#13529=DIRECTION('',(0.,0.,1.));
#13530=DIRECTION('',(1.,0.,0.));
#13531=CARTESIAN_POINT('',(0.,0.,0.));
#13532=CARTESIAN_POINT('',(0.,0.,0.));
#13533=CARTESIAN_POINT('',(0.,0.,0.));
#13534=CARTESIAN_POINT('Origin',(2.9,17.5,-0.1));
#13535=CARTESIAN_POINT('',(2.735,17.5,0.));
#13536=CARTESIAN_POINT('Origin',(2.9,17.5,0.));
#13537=CARTESIAN_POINT('',(2.735,17.5,1.));
#13538=CARTESIAN_POINT('',(2.735,17.5,-0.1));
#13539=CARTESIAN_POINT('Origin',(2.9,17.5,1.));
#13540=CARTESIAN_POINT('Origin',(5.1,17.5,-0.1));
#13541=CARTESIAN_POINT('',(4.935,17.5,0.));
#13542=CARTESIAN_POINT('Origin',(5.1,17.5,0.));
#13543=CARTESIAN_POINT('',(4.935,17.5,1.));
#13544=CARTESIAN_POINT('',(4.935,17.5,-0.1));
#13545=CARTESIAN_POINT('Origin',(5.1,17.5,1.));
#13546=CARTESIAN_POINT('Origin',(2.9,7.5,-0.1));
#13547=CARTESIAN_POINT('',(2.735,7.5,0.));
#13548=CARTESIAN_POINT('Origin',(2.9,7.5,0.));
#13549=CARTESIAN_POINT('',(2.735,7.5,1.));
#13550=CARTESIAN_POINT('',(2.735,7.5,-0.1));
#13551=CARTESIAN_POINT('Origin',(2.9,7.5,1.));
#13552=CARTESIAN_POINT('Origin',(5.1,7.5,-0.1));
#13553=CARTESIAN_POINT('',(4.935,7.5,0.));
#13554=CARTESIAN_POINT('Origin',(5.1,7.5,0.));
#13555=CARTESIAN_POINT('',(4.935,7.5,1.));
#13556=CARTESIAN_POINT('',(4.935,7.5,-0.1));
#13557=CARTESIAN_POINT('Origin',(5.1,7.5,1.));
#13558=CARTESIAN_POINT('Origin',(15.5,0.9,-0.1));
#13559=CARTESIAN_POINT('',(15.335,0.9,0.));
#13560=CARTESIAN_POINT('Origin',(15.5,0.9,0.));
#13561=CARTESIAN_POINT('',(15.335,0.9,1.));
#13562=CARTESIAN_POINT('',(15.335,0.9,-0.1));
#13563=CARTESIAN_POINT('Origin',(15.5,0.9,1.));
#13564=CARTESIAN_POINT('Origin',(15.5,3.1,-0.1));
#13565=CARTESIAN_POINT('',(15.335,3.1,0.));
#13566=CARTESIAN_POINT('Origin',(15.5,3.1,0.));
#13567=CARTESIAN_POINT('',(15.335,3.1,1.));
#13568=CARTESIAN_POINT('',(15.335,3.1,-0.1));
#13569=CARTESIAN_POINT('Origin',(15.5,3.1,1.));
#13570=CARTESIAN_POINT('Origin',(5.5,0.9,-0.1));
#13571=CARTESIAN_POINT('',(5.335,0.9,0.));
#13572=CARTESIAN_POINT('Origin',(5.5,0.9,0.));
#13573=CARTESIAN_POINT('',(5.335,0.9,1.));
#13574=CARTESIAN_POINT('',(5.335,0.9,-0.1));
#13575=CARTESIAN_POINT('Origin',(5.5,0.9,1.));
#13576=CARTESIAN_POINT('Origin',(5.5,3.1,-0.1));
#13577=CARTESIAN_POINT('',(5.335,3.1,0.));
#13578=CARTESIAN_POINT('Origin',(5.5,3.1,0.));
#13579=CARTESIAN_POINT('',(5.335,3.1,1.));
#13580=CARTESIAN_POINT('',(5.335,3.1,-0.1));
#13581=CARTESIAN_POINT('Origin',(5.5,3.1,1.));
#13582=CARTESIAN_POINT('Origin',(-1.76776695296637,-1.76776695296637,-0.1));
#13583=CARTESIAN_POINT('',(-1.97776695296637,-1.76776695296637,0.));
#13584=CARTESIAN_POINT('Origin',(-1.76776695296637,-1.76776695296637,0.));
#13585=CARTESIAN_POINT('',(-1.97776695296637,-1.76776695296637,1.));
#13586=CARTESIAN_POINT('',(-1.97776695296637,-1.76776695296637,-0.1));
#13587=CARTESIAN_POINT('Origin',(-1.76776695296637,-1.76776695296637,1.));
#13588=CARTESIAN_POINT('Origin',(-1.76776695296637,1.76776695296637,-0.1));
#13589=CARTESIAN_POINT('',(-1.97776695296637,1.76776695296637,0.));
#13590=CARTESIAN_POINT('Origin',(-1.76776695296637,1.76776695296637,0.));
#13591=CARTESIAN_POINT('',(-1.97776695296637,1.76776695296637,1.));
#13592=CARTESIAN_POINT('',(-1.97776695296637,1.76776695296637,-0.1));
#13593=CARTESIAN_POINT('Origin',(-1.76776695296637,1.76776695296637,1.));
#13594=CARTESIAN_POINT('Origin',(1.76776695296637,1.76776695296637,-0.1));
#13595=CARTESIAN_POINT('',(1.55776695296637,1.76776695296637,0.));
#13596=CARTESIAN_POINT('Origin',(1.76776695296637,1.76776695296637,0.));
#13597=CARTESIAN_POINT('',(1.55776695296637,1.76776695296637,1.));
#13598=CARTESIAN_POINT('',(1.55776695296637,1.76776695296637,-0.1));
#13599=CARTESIAN_POINT('Origin',(1.76776695296637,1.76776695296637,1.));
#13600=CARTESIAN_POINT('Origin',(1.76776695296637,-1.76776695296637,-0.1));
#13601=CARTESIAN_POINT('',(1.55776695296637,-1.76776695296637,0.));
#13602=CARTESIAN_POINT('Origin',(1.76776695296637,-1.76776695296637,0.));
#13603=CARTESIAN_POINT('',(1.55776695296637,-1.76776695296637,1.));
#13604=CARTESIAN_POINT('',(1.55776695296637,-1.76776695296637,-0.1));
#13605=CARTESIAN_POINT('Origin',(1.76776695296637,-1.76776695296637,1.));
#13606=CARTESIAN_POINT('Origin',(17.,19.,0.));
#13607=CARTESIAN_POINT('',(17.,19.,0.));
#13608=CARTESIAN_POINT('',(-4.,19.,0.));
#13609=CARTESIAN_POINT('',(17.,19.,0.));
#13610=CARTESIAN_POINT('',(-4.,19.,1.));
#13611=CARTESIAN_POINT('',(-4.,19.,0.));
#13612=CARTESIAN_POINT('',(17.,19.,1.));
#13613=CARTESIAN_POINT('',(17.,19.,1.));
#13614=CARTESIAN_POINT('',(17.,19.,0.));
#13615=CARTESIAN_POINT('Origin',(17.,-4.,0.));
#13616=CARTESIAN_POINT('',(17.,-4.,0.));
#13617=CARTESIAN_POINT('',(17.,-4.,0.));
#13618=CARTESIAN_POINT('',(17.,-4.,1.));
#13619=CARTESIAN_POINT('',(17.,-4.,1.));
#13620=CARTESIAN_POINT('',(17.,-4.,0.));
#13621=CARTESIAN_POINT('Origin',(-4.,-4.,0.));
#13622=CARTESIAN_POINT('',(-4.,-4.,0.));
#13623=CARTESIAN_POINT('',(-4.,-4.,0.));
#13624=CARTESIAN_POINT('',(-4.,-4.,1.));
#13625=CARTESIAN_POINT('',(-4.,-4.,1.));
#13626=CARTESIAN_POINT('',(-4.,-4.,0.));
#13627=CARTESIAN_POINT('Origin',(-4.,19.,0.));
#13628=CARTESIAN_POINT('',(-4.,19.,0.));
#13629=CARTESIAN_POINT('',(-4.,19.,1.));
#13630=CARTESIAN_POINT('Origin',(6.5,7.5,1.));
#13631=CARTESIAN_POINT('Origin',(6.5,7.5,0.));
#13632=CARTESIAN_POINT('',(0.,0.,0.));
#13633=CARTESIAN_POINT('Origin',(-3.,19.,-0.8));
#13634=CARTESIAN_POINT('',(-3.,19.,-0.8));
#13635=CARTESIAN_POINT('',(-4.,19.,-0.8));
#13636=CARTESIAN_POINT('',(-3.,19.,-0.8));
#13637=CARTESIAN_POINT('',(-4.,19.,0.));
#13638=CARTESIAN_POINT('',(-4.,19.,-0.8));
#13639=CARTESIAN_POINT('',(-3.,19.,0.));
#13640=CARTESIAN_POINT('',(-3.,19.,0.));
#13641=CARTESIAN_POINT('',(-3.,19.,-0.8));
#13642=CARTESIAN_POINT('Origin',(-3.,-4.,-0.8));
#13643=CARTESIAN_POINT('',(-3.,-4.,-0.8));
#13644=CARTESIAN_POINT('',(-3.,-4.,-0.8));
#13645=CARTESIAN_POINT('',(-3.,-4.,0.));
#13646=CARTESIAN_POINT('',(-3.,-4.,0.));
#13647=CARTESIAN_POINT('',(-3.,-4.,-0.8));
#13648=CARTESIAN_POINT('Origin',(-4.,-4.,-0.8));
#13649=CARTESIAN_POINT('',(-4.,-4.,-0.8));
#13650=CARTESIAN_POINT('',(-4.,-4.,-0.8));
#13651=CARTESIAN_POINT('',(-4.,-4.,0.));
#13652=CARTESIAN_POINT('',(-4.,-4.,0.));
#13653=CARTESIAN_POINT('',(-4.,-4.,-0.8));
#13654=CARTESIAN_POINT('Origin',(-4.,19.,-0.8));
#13655=CARTESIAN_POINT('',(-4.,19.,-0.8));
#13656=CARTESIAN_POINT('',(-4.,19.,0.));
#13657=CARTESIAN_POINT('Origin',(-3.5,7.5,0.));
#13658=CARTESIAN_POINT('Origin',(-3.5,7.5,-0.8));
#13659=CARTESIAN_POINT('',(0.,0.,0.));
#13660=CARTESIAN_POINT('Origin',(17.,19.,-0.8));
#13661=CARTESIAN_POINT('',(17.,19.,-0.8));
#13662=CARTESIAN_POINT('',(16.,19.,-0.8));
#13663=CARTESIAN_POINT('',(17.,19.,-0.8));
#13664=CARTESIAN_POINT('',(16.,19.,0.));
#13665=CARTESIAN_POINT('',(16.,19.,-0.8));
#13666=CARTESIAN_POINT('',(17.,19.,0.));
#13667=CARTESIAN_POINT('',(17.,19.,0.));
#13668=CARTESIAN_POINT('',(17.,19.,-0.8));
#13669=CARTESIAN_POINT('Origin',(17.,-4.,-0.8));
#13670=CARTESIAN_POINT('',(17.,-4.,-0.8));
#13671=CARTESIAN_POINT('',(17.,-4.,-0.8));
#13672=CARTESIAN_POINT('',(17.,-4.,0.));
#13673=CARTESIAN_POINT('',(17.,-4.,0.));
#13674=CARTESIAN_POINT('',(17.,-4.,-0.8));
#13675=CARTESIAN_POINT('Origin',(16.,-4.,-0.8));
#13676=CARTESIAN_POINT('',(16.,-4.,-0.8));
#13677=CARTESIAN_POINT('',(16.,-4.,-0.8));
#13678=CARTESIAN_POINT('',(16.,-4.,0.));
#13679=CARTESIAN_POINT('',(16.,-4.,0.));
#13680=CARTESIAN_POINT('',(16.,-4.,-0.8));
#13681=CARTESIAN_POINT('Origin',(16.,19.,-0.8));
#13682=CARTESIAN_POINT('',(16.,19.,-0.8));
#13683=CARTESIAN_POINT('',(16.,19.,0.));
#13684=CARTESIAN_POINT('Origin',(16.5,7.5,0.));
#13685=CARTESIAN_POINT('Origin',(16.5,7.5,-0.8));
#13686=CARTESIAN_POINT('',(0.,0.,0.));
#13687=CARTESIAN_POINT('Origin',(0.9,0.,1.4));
#13688=CARTESIAN_POINT('',(0.988888264668966,0.25,1.4));
#13689=CARTESIAN_POINT('',(1.02,-1.18386380373883E-17,1.65));
#13690=CARTESIAN_POINT('Ctrl Pts',(0.988888264668966,0.25,1.4));
#13691=CARTESIAN_POINT('Ctrl Pts',(0.988888264668966,0.25,1.43153139415882));
#13692=CARTESIAN_POINT('Ctrl Pts',(0.990553370646674,0.243672048431404,
1.46507214966317));
#13693=CARTESIAN_POINT('Ctrl Pts',(0.996491737296663,0.218119830014375,
1.52662620974954));
#13694=CARTESIAN_POINT('Ctrl Pts',(1.00067109353237,0.198902128206072,1.5546512623872));
#13695=CARTESIAN_POINT('Ctrl Pts',(1.00845756932386,0.154654113568716,1.59889927702456));
#13696=CARTESIAN_POINT('Ctrl Pts',(1.01258144235289,0.126627870945253,1.61811920309393));
#13697=CARTESIAN_POINT('Ctrl Pts',(1.0183917429657,0.065069600391363,1.64367304400768));
#13698=CARTESIAN_POINT('Ctrl Pts',(1.02,0.031527330883376,1.65));
#13699=CARTESIAN_POINT('Ctrl Pts',(1.02,2.77555756156289E-17,1.65));
#13700=CARTESIAN_POINT('Ctrl Pts',(1.02,6.93889390390723E-18,1.65));
#13701=CARTESIAN_POINT('Ctrl Pts',(1.02,-0.031527330883376,1.65));
#13702=CARTESIAN_POINT('Ctrl Pts',(1.0183917429657,-0.065069600391363,1.64367304400768));
#13703=CARTESIAN_POINT('Ctrl Pts',(1.01258144235289,-0.126627870945253,
1.61811920309393));
#13704=CARTESIAN_POINT('Ctrl Pts',(1.00845756932386,-0.154654113568716,
1.59889927702456));
#13705=CARTESIAN_POINT('Ctrl Pts',(1.00067109353237,-0.198902128206072,
1.5546512623872));
#13706=CARTESIAN_POINT('Ctrl Pts',(0.996491737296663,-0.218119830014375,
1.52662620974954));
#13707=CARTESIAN_POINT('Ctrl Pts',(0.990553370646674,-0.243672048431404,
1.46507214966317));
#13708=CARTESIAN_POINT('Ctrl Pts',(0.988888264668967,-0.25,1.43153139415882));
#13709=CARTESIAN_POINT('Ctrl Pts',(0.988888264668967,-0.25,1.36846860584118));
#13710=CARTESIAN_POINT('Ctrl Pts',(0.990553370646674,-0.243672048431404,
1.33492785033683));
#13711=CARTESIAN_POINT('Ctrl Pts',(0.996491737296663,-0.218119830014375,
1.27337379025046));
#13712=CARTESIAN_POINT('Ctrl Pts',(1.00067109353237,-0.198902128206072,
1.2453487376128));
#13713=CARTESIAN_POINT('Ctrl Pts',(1.00845756932386,-0.154654113568716,
1.20110072297544));
#13714=CARTESIAN_POINT('Ctrl Pts',(1.01258144235289,-0.126627870945254,
1.18188079690607));
#13715=CARTESIAN_POINT('Ctrl Pts',(1.0183917429657,-0.0650696003913633,
1.15632695599232));
#13716=CARTESIAN_POINT('Ctrl Pts',(1.02,-0.0315273308833761,1.15));
#13717=CARTESIAN_POINT('Ctrl Pts',(1.02,0.0315273308833759,1.15));
#13718=CARTESIAN_POINT('Ctrl Pts',(1.0183917429657,0.065069600391363,1.15632695599232));
#13719=CARTESIAN_POINT('Ctrl Pts',(1.01258144235289,0.126627870945253,1.18188079690607));
#13720=CARTESIAN_POINT('Ctrl Pts',(1.00845756932386,0.154654113568716,1.20110072297544));
#13721=CARTESIAN_POINT('Ctrl Pts',(1.00067109353237,0.198902128206072,1.2453487376128));
#13722=CARTESIAN_POINT('Ctrl Pts',(0.996491737296663,0.218119830014375,
1.27337379025046));
#13723=CARTESIAN_POINT('Ctrl Pts',(0.990553370646674,0.243672048431404,
1.33492785033683));
#13724=CARTESIAN_POINT('Ctrl Pts',(0.988888264668967,0.25,1.36846860584118));
#13725=CARTESIAN_POINT('Ctrl Pts',(0.988888264668967,0.25,1.4));
#13726=CARTESIAN_POINT('',(3.,-3.06161699786838E-17,1.65));
#13727=CARTESIAN_POINT('',(0.9,-3.06161699786838E-17,1.65));
#13728=CARTESIAN_POINT('',(2.98956518577535,0.25,1.4));
#13729=CARTESIAN_POINT('Ctrl Pts',(2.98956518577535,0.25,1.4));
#13730=CARTESIAN_POINT('Ctrl Pts',(2.98956518577535,0.25,1.36859378633186));
#13731=CARTESIAN_POINT('Ctrl Pts',(2.99011104995181,0.24372047740942,1.33510417960069));
#13732=CARTESIAN_POINT('Ctrl Pts',(2.99208145165098,0.218202539734559,1.27351367328886));
#13733=CARTESIAN_POINT('Ctrl Pts',(2.99347740802958,0.198964922639276,1.245411532046));
#13734=CARTESIAN_POINT('Ctrl Pts',(2.99609686518216,0.154588504271054,1.20103511367778));
#13735=CARTESIAN_POINT('Ctrl Pts',(2.99749070376198,0.126486346986081,1.18179746841036));
#13736=CARTESIAN_POINT('Ctrl Pts',(2.99945625936844,0.0648957875009219,
1.15627950921557));
#13737=CARTESIAN_POINT('Ctrl Pts',(3.,0.0314061622633416,1.15));
#13738=CARTESIAN_POINT('Ctrl Pts',(3.,-0.0314061622633416,1.15));
#13739=CARTESIAN_POINT('Ctrl Pts',(2.99945625936844,-0.0648957875009221,
1.15627950921557));
#13740=CARTESIAN_POINT('Ctrl Pts',(2.99749070376198,-0.126486346986081,
1.18179746841036));
#13741=CARTESIAN_POINT('Ctrl Pts',(2.99609686518216,-0.154588504271054,
1.20103511367778));
#13742=CARTESIAN_POINT('Ctrl Pts',(2.99347740802958,-0.198964922639276,
1.245411532046));
#13743=CARTESIAN_POINT('Ctrl Pts',(2.99208145165098,-0.218202539734559,
1.27351367328886));
#13744=CARTESIAN_POINT('Ctrl Pts',(2.99011104995181,-0.24372047740942,1.33510417960069));
#13745=CARTESIAN_POINT('Ctrl Pts',(2.98956518577535,-0.25,1.36859378633186));
#13746=CARTESIAN_POINT('Ctrl Pts',(2.98956518577535,-0.25,1.43140621366814));
#13747=CARTESIAN_POINT('Ctrl Pts',(2.99011104995181,-0.24372047740942,1.4648958203993));
#13748=CARTESIAN_POINT('Ctrl Pts',(2.99208145165098,-0.21820253973456,1.52648632671114));
#13749=CARTESIAN_POINT('Ctrl Pts',(2.99347740802958,-0.198964922639276,
1.554588467954));
#13750=CARTESIAN_POINT('Ctrl Pts',(2.99609686518216,-0.154588504271054,
1.59896488632222));
#13751=CARTESIAN_POINT('Ctrl Pts',(2.99749070376198,-0.126486346986082,
1.61820253158964));
#13752=CARTESIAN_POINT('Ctrl Pts',(2.99945625936844,-0.0648957875009221,
1.64372049078443));
#13753=CARTESIAN_POINT('Ctrl Pts',(3.,-0.0314061622633417,1.65));
#13754=CARTESIAN_POINT('Ctrl Pts',(3.,-5.55111512312578E-17,1.65));
#13755=CARTESIAN_POINT('Ctrl Pts',(3.,-2.08166817117217E-17,1.65));
#13756=CARTESIAN_POINT('Ctrl Pts',(3.,0.0314061622633416,1.65));
#13757=CARTESIAN_POINT('Ctrl Pts',(2.99945625936844,0.0648957875009221,
1.64372049078443));
#13758=CARTESIAN_POINT('Ctrl Pts',(2.99749070376198,0.126486346986081,1.61820253158964));
#13759=CARTESIAN_POINT('Ctrl Pts',(2.99609686518216,0.154588504271054,1.59896488632222));
#13760=CARTESIAN_POINT('Ctrl Pts',(2.99347740802958,0.198964922639276,1.554588467954));
#13761=CARTESIAN_POINT('Ctrl Pts',(2.99208145165098,0.218202539734559,1.52648632671114));
#13762=CARTESIAN_POINT('Ctrl Pts',(2.99011104995181,0.24372047740942,1.46489582039931));
#13763=CARTESIAN_POINT('Ctrl Pts',(2.98956518577535,0.25,1.43140621366814));
#13764=CARTESIAN_POINT('Ctrl Pts',(2.98956518577535,0.25,1.4));
#13765=CARTESIAN_POINT('Origin',(-1.23743686707646,-1.23743686707646,2.9));
#13766=CARTESIAN_POINT('',(-1.40243686707646,-1.23743686707646,2.9));
#13767=CARTESIAN_POINT('Origin',(-1.23743686707646,-1.23743686707646,2.9));
#13768=CARTESIAN_POINT('',(-1.40243686707646,-1.23743686707646,3.6));
#13769=CARTESIAN_POINT('',(-1.40243686707646,-1.23743686707646,2.9));
#13770=CARTESIAN_POINT('Origin',(-1.23743686707646,-1.23743686707646,3.6));
#13771=CARTESIAN_POINT('Origin',(-1.23743686707646,-1.23743686707646,2.9));
#13772=CARTESIAN_POINT('Origin',(-1.23743686707646,1.23743686707646,2.9));
#13773=CARTESIAN_POINT('',(-1.40243686707646,1.23743686707646,2.9));
#13774=CARTESIAN_POINT('Origin',(-1.23743686707646,1.23743686707646,2.9));
#13775=CARTESIAN_POINT('',(-1.40243686707646,1.23743686707646,3.6));
#13776=CARTESIAN_POINT('',(-1.40243686707646,1.23743686707646,2.9));
#13777=CARTESIAN_POINT('Origin',(-1.23743686707646,1.23743686707646,3.6));
#13778=CARTESIAN_POINT('Origin',(-1.23743686707646,1.23743686707646,2.9));
#13779=CARTESIAN_POINT('Origin',(1.23743686707646,1.23743686707646,2.9));
#13780=CARTESIAN_POINT('',(1.07243686707646,1.23743686707646,2.9));
#13781=CARTESIAN_POINT('Origin',(1.23743686707646,1.23743686707646,2.9));
#13782=CARTESIAN_POINT('',(1.07243686707646,1.23743686707646,3.6));
#13783=CARTESIAN_POINT('',(1.07243686707646,1.23743686707646,2.9));
#13784=CARTESIAN_POINT('Origin',(1.23743686707646,1.23743686707646,3.6));
#13785=CARTESIAN_POINT('Origin',(1.23743686707646,1.23743686707646,2.9));
#13786=CARTESIAN_POINT('Origin',(1.23743686707646,-1.23743686707646,2.9));
#13787=CARTESIAN_POINT('',(1.07243686707646,-1.23743686707646,2.9));
#13788=CARTESIAN_POINT('Origin',(1.23743686707646,-1.23743686707646,2.9));
#13789=CARTESIAN_POINT('',(1.07243686707646,-1.23743686707646,3.6));
#13790=CARTESIAN_POINT('',(1.07243686707646,-1.23743686707646,2.9));
#13791=CARTESIAN_POINT('Origin',(1.23743686707646,-1.23743686707646,3.6));
#13792=CARTESIAN_POINT('Origin',(1.23743686707646,-1.23743686707646,2.9));
#13793=CARTESIAN_POINT('Origin',(-1.76776695296637,-1.76776695296637,2.4));
#13794=CARTESIAN_POINT('',(-1.8139637388702,-1.24480341984751,2.4));
#13795=CARTESIAN_POINT('',(-1.24480341984751,-1.81396373887019,2.4));
#13796=CARTESIAN_POINT('Origin',(0.,0.,2.4));
#13797=CARTESIAN_POINT('Origin',(-1.76776695296637,-1.76776695296637,2.4));
#13798=CARTESIAN_POINT('Origin',(-1.76776695296637,-1.76776695296637,1.8));
#13799=CARTESIAN_POINT('',(-1.8139637388702,-1.24480341984751,1.8));
#13800=CARTESIAN_POINT('',(-1.8139637388702,-1.24480341984751,1.8));
#13801=CARTESIAN_POINT('',(-1.24480341984751,-1.81396373887019,1.8));
#13802=CARTESIAN_POINT('Origin',(-1.76776695296637,-1.76776695296637,1.8));
#13803=CARTESIAN_POINT('',(-1.24480341984751,-1.81396373887019,1.8));
#13804=CARTESIAN_POINT('Origin',(-1.76776695296637,1.76776695296637,1.8));
#13805=CARTESIAN_POINT('',(-1.81396373887019,1.24480341984751,2.4));
#13806=CARTESIAN_POINT('',(-1.81396373887019,1.24480341984751,1.8));
#13807=CARTESIAN_POINT('',(-1.81396373887019,1.24480341984751,1.8));
#13808=CARTESIAN_POINT('',(-1.24480341984751,1.81396373887019,2.4));
#13809=CARTESIAN_POINT('Origin',(-1.76776695296637,1.76776695296637,2.4));
#13810=CARTESIAN_POINT('',(-1.24480341984751,1.81396373887019,1.8));
#13811=CARTESIAN_POINT('',(-1.24480341984751,1.81396373887019,1.8));
#13812=CARTESIAN_POINT('Origin',(-1.76776695296637,1.76776695296637,1.8));
#13813=CARTESIAN_POINT('Origin',(-1.76776695296637,1.76776695296637,2.4));
#13814=CARTESIAN_POINT('Origin',(0.,0.,2.4));
#13815=CARTESIAN_POINT('Origin',(1.76776695296637,1.76776695296637,1.8));
#13816=CARTESIAN_POINT('',(1.24480341984751,1.81396373887019,2.4));
#13817=CARTESIAN_POINT('',(1.24480341984751,1.81396373887019,1.8));
#13818=CARTESIAN_POINT('',(1.24480341984751,1.81396373887019,1.8));
#13819=CARTESIAN_POINT('',(1.81396373887019,1.24480341984751,2.4));
#13820=CARTESIAN_POINT('Origin',(1.76776695296637,1.76776695296637,2.4));
#13821=CARTESIAN_POINT('',(1.81396373887019,1.24480341984751,1.8));
#13822=CARTESIAN_POINT('',(1.81396373887019,1.24480341984751,1.8));
#13823=CARTESIAN_POINT('Origin',(1.76776695296637,1.76776695296637,1.8));
#13824=CARTESIAN_POINT('Origin',(1.76776695296637,1.76776695296637,2.4));
#13825=CARTESIAN_POINT('Origin',(0.,0.,2.4));
#13826=CARTESIAN_POINT('Origin',(1.76776695296637,-1.76776695296637,1.8));
#13827=CARTESIAN_POINT('',(1.81396373887019,-1.24480341984751,2.4));
#13828=CARTESIAN_POINT('',(1.81396373887019,-1.24480341984751,1.8));
#13829=CARTESIAN_POINT('',(1.81396373887019,-1.24480341984751,1.8));
#13830=CARTESIAN_POINT('',(1.24480341984751,-1.8139637388702,2.4));
#13831=CARTESIAN_POINT('Origin',(1.76776695296637,-1.76776695296637,2.4));
#13832=CARTESIAN_POINT('',(1.24480341984751,-1.8139637388702,1.8));
#13833=CARTESIAN_POINT('',(1.24480341984751,-1.8139637388702,1.8));
#13834=CARTESIAN_POINT('Origin',(1.76776695296637,-1.76776695296637,1.8));
#13835=CARTESIAN_POINT('Origin',(1.76776695296637,-1.76776695296637,2.4));
#13836=CARTESIAN_POINT('Origin',(0.,0.,2.4));
#13837=CARTESIAN_POINT('Origin',(0.,0.,1.));
#13838=CARTESIAN_POINT('',(-2.2,-2.69422295812418E-16,3.6));
#13839=CARTESIAN_POINT('Origin',(0.,0.,3.6));
#13840=CARTESIAN_POINT('',(-2.2,-2.69422295812418E-16,1.8));
#13841=CARTESIAN_POINT('',(-2.2,-2.69422295812418E-16,1.));
#13842=CARTESIAN_POINT('Origin',(0.,0.,1.8));
#13843=CARTESIAN_POINT('Origin',(0.,0.,1.8));
#13844=CARTESIAN_POINT('Origin',(0.,0.,1.8));
#13845=CARTESIAN_POINT('Origin',(0.,0.,1.8));
#13846=CARTESIAN_POINT('Origin',(0.,0.,1.8));
#13847=CARTESIAN_POINT('Origin',(0.,0.,1.8));
#13848=CARTESIAN_POINT('',(-3.,-3.67394039744206E-16,1.8));
#13849=CARTESIAN_POINT('Origin',(0.,0.,1.8));
#13850=CARTESIAN_POINT('',(-2.04276695296637,-1.76776695296637,1.8));
#13851=CARTESIAN_POINT('Origin',(-1.76776695296637,-1.76776695296637,1.8));
#13852=CARTESIAN_POINT('',(1.49276695296637,1.76776695296637,1.8));
#13853=CARTESIAN_POINT('Origin',(1.76776695296637,1.76776695296637,1.8));
#13854=CARTESIAN_POINT('',(1.49276695296637,-1.76776695296637,1.8));
#13855=CARTESIAN_POINT('Origin',(1.76776695296637,-1.76776695296637,1.8));
#13856=CARTESIAN_POINT('',(-2.04276695296637,1.76776695296637,1.8));
#13857=CARTESIAN_POINT('Origin',(-1.76776695296637,1.76776695296637,1.8));
#13858=CARTESIAN_POINT('Origin',(-1.76776695296637,-1.76776695296637,0.9));
#13859=CARTESIAN_POINT('',(-2.04276695296637,-1.76776695296637,1.));
#13860=CARTESIAN_POINT('Origin',(-1.76776695296637,-1.76776695296637,1.));
#13861=CARTESIAN_POINT('',(-2.04276695296637,-1.76776695296637,0.9));
#13862=CARTESIAN_POINT('Origin',(-1.76776695296637,1.76776695296637,0.9));
#13863=CARTESIAN_POINT('',(-2.04276695296637,1.76776695296637,1.));
#13864=CARTESIAN_POINT('Origin',(-1.76776695296637,1.76776695296637,1.));
#13865=CARTESIAN_POINT('',(-2.04276695296637,1.76776695296637,0.9));
#13866=CARTESIAN_POINT('Origin',(1.76776695296637,1.76776695296637,0.9));
#13867=CARTESIAN_POINT('',(1.49276695296637,1.76776695296637,1.));
#13868=CARTESIAN_POINT('Origin',(1.76776695296637,1.76776695296637,1.));
#13869=CARTESIAN_POINT('',(1.49276695296637,1.76776695296637,0.9));
#13870=CARTESIAN_POINT('Origin',(1.76776695296637,-1.76776695296637,0.9));
#13871=CARTESIAN_POINT('',(1.49276695296637,-1.76776695296637,1.));
#13872=CARTESIAN_POINT('Origin',(1.76776695296637,-1.76776695296637,1.));
#13873=CARTESIAN_POINT('',(1.49276695296637,-1.76776695296637,0.9));
#13874=CARTESIAN_POINT('Origin',(0.,0.,2.05));
#13875=CARTESIAN_POINT('',(-1.5,-1.83697019872103E-16,2.05));
#13876=CARTESIAN_POINT('Origin',(0.,0.,2.05));
#13877=CARTESIAN_POINT('',(-1.5,1.83697019872103E-16,3.6));
#13878=CARTESIAN_POINT('',(-1.5,-1.83697019872103E-16,2.05));
#13879=CARTESIAN_POINT('Origin',(0.,0.,3.6));
#13880=CARTESIAN_POINT('Origin',(0.,0.,2.05));
#13881=CARTESIAN_POINT('',(-1.02,-1.2491397351303E-16,2.05));
#13882=CARTESIAN_POINT('Origin',(0.,0.,2.05));
#13883=CARTESIAN_POINT('Origin',(0.,0.,1.));
#13884=CARTESIAN_POINT('',(-3.,-3.67394039744206E-16,1.));
#13885=CARTESIAN_POINT('',(-3.,-3.67394039744206E-16,1.));
#13886=CARTESIAN_POINT('Origin',(0.,0.,1.));
#13887=CARTESIAN_POINT('Origin',(0.,0.,1.));
#13888=CARTESIAN_POINT('',(-1.02,-1.2491397351303E-16,1.));
#13889=CARTESIAN_POINT('',(-1.02,-1.2491397351303E-16,1.));
#13890=CARTESIAN_POINT('Origin',(0.,0.,1.));
#13891=CARTESIAN_POINT('Origin',(0.,0.,3.6));
#13892=CARTESIAN_POINT('Origin',(0.,0.,1.));
#13893=CARTESIAN_POINT('',(0.,0.,0.));
#13894=CARTESIAN_POINT('Origin',(-1.23743686707646,-1.23743686707646,4.));
#13895=CARTESIAN_POINT('',(-1.61243686707646,-1.23743686707646,4.));
#13896=CARTESIAN_POINT('Origin',(-1.23743686707646,-1.23743686707646,4.));
#13897=CARTESIAN_POINT('',(-1.61243686707646,-1.23743686707646,4.4));
#13898=CARTESIAN_POINT('',(-1.61243686707646,-1.23743686707646,4.));
#13899=CARTESIAN_POINT('Origin',(-1.23743686707646,-1.23743686707646,4.4));
#13900=CARTESIAN_POINT('Origin',(-1.23743686707646,-1.23743686707646,4.));
#13901=CARTESIAN_POINT('',(-1.46243686707646,-1.23743686707646,4.));
#13902=CARTESIAN_POINT('Origin',(-1.23743686707646,-1.23743686707646,4.));
#13903=CARTESIAN_POINT('Origin',(-1.23743686707646,1.23743686707646,4.));
#13904=CARTESIAN_POINT('',(-1.61243686707646,1.23743686707646,4.));
#13905=CARTESIAN_POINT('Origin',(-1.23743686707646,1.23743686707646,4.));
#13906=CARTESIAN_POINT('',(-1.61243686707646,1.23743686707646,4.4));
#13907=CARTESIAN_POINT('',(-1.61243686707646,1.23743686707646,4.));
#13908=CARTESIAN_POINT('Origin',(-1.23743686707646,1.23743686707646,4.4));
#13909=CARTESIAN_POINT('Origin',(-1.23743686707646,1.23743686707646,4.));
#13910=CARTESIAN_POINT('',(-1.46243686707646,1.23743686707646,4.));
#13911=CARTESIAN_POINT('Origin',(-1.23743686707646,1.23743686707646,4.));
#13912=CARTESIAN_POINT('Origin',(1.23743686707646,1.23743686707646,4.));
#13913=CARTESIAN_POINT('',(0.862436867076458,1.23743686707646,4.));
#13914=CARTESIAN_POINT('Origin',(1.23743686707646,1.23743686707646,4.));
#13915=CARTESIAN_POINT('',(0.862436867076458,1.23743686707646,4.4));
#13916=CARTESIAN_POINT('',(0.862436867076458,1.23743686707646,4.));
#13917=CARTESIAN_POINT('Origin',(1.23743686707646,1.23743686707646,4.4));
#13918=CARTESIAN_POINT('Origin',(1.23743686707646,1.23743686707646,4.));
#13919=CARTESIAN_POINT('',(1.01243686707646,1.23743686707646,4.));
#13920=CARTESIAN_POINT('Origin',(1.23743686707646,1.23743686707646,4.));
#13921=CARTESIAN_POINT('Origin',(1.23743686707646,-1.23743686707646,4.));
#13922=CARTESIAN_POINT('',(0.862436867076458,-1.23743686707646,4.));
#13923=CARTESIAN_POINT('Origin',(1.23743686707646,-1.23743686707646,4.));
#13924=CARTESIAN_POINT('',(0.862436867076458,-1.23743686707646,4.4));
#13925=CARTESIAN_POINT('',(0.862436867076458,-1.23743686707646,4.));
#13926=CARTESIAN_POINT('Origin',(1.23743686707646,-1.23743686707646,4.4));
#13927=CARTESIAN_POINT('Origin',(1.23743686707646,-1.23743686707646,4.));
#13928=CARTESIAN_POINT('',(1.01243686707646,-1.23743686707646,4.));
#13929=CARTESIAN_POINT('Origin',(1.23743686707646,-1.23743686707646,4.));
#13930=CARTESIAN_POINT('Origin',(-1.23743686707646,-1.23743686707646,3.5));
#13931=CARTESIAN_POINT('',(-1.46243686707646,-1.23743686707646,3.6));
#13932=CARTESIAN_POINT('Origin',(-1.23743686707646,-1.23743686707646,3.6));
#13933=CARTESIAN_POINT('',(-1.46243686707646,-1.23743686707646,3.5));
#13934=CARTESIAN_POINT('Origin',(-1.23743686707646,1.23743686707646,3.5));
#13935=CARTESIAN_POINT('',(-1.46243686707646,1.23743686707646,3.6));
#13936=CARTESIAN_POINT('Origin',(-1.23743686707646,1.23743686707646,3.6));
#13937=CARTESIAN_POINT('',(-1.46243686707646,1.23743686707646,3.5));
#13938=CARTESIAN_POINT('Origin',(1.23743686707646,1.23743686707646,3.5));
#13939=CARTESIAN_POINT('',(1.01243686707646,1.23743686707646,3.6));
#13940=CARTESIAN_POINT('Origin',(1.23743686707646,1.23743686707646,3.6));
#13941=CARTESIAN_POINT('',(1.01243686707646,1.23743686707646,3.5));
#13942=CARTESIAN_POINT('Origin',(1.23743686707646,-1.23743686707646,3.5));
#13943=CARTESIAN_POINT('',(1.01243686707646,-1.23743686707646,3.6));
#13944=CARTESIAN_POINT('Origin',(1.23743686707646,-1.23743686707646,3.6));
#13945=CARTESIAN_POINT('',(1.01243686707646,-1.23743686707646,3.5));
#13946=CARTESIAN_POINT('Origin',(0.,0.,2.95));
#13947=CARTESIAN_POINT('',(-1.49,-1.82472373072956E-16,3.6));
#13948=CARTESIAN_POINT('Origin',(0.,0.,3.6));
#13949=CARTESIAN_POINT('',(-1.49,-1.82472373072956E-16,2.95));
#13950=CARTESIAN_POINT('',(-1.49,-1.82472373072956E-16,2.95));
#13951=CARTESIAN_POINT('Origin',(0.,0.,2.95));
#13952=CARTESIAN_POINT('Origin',(0.,0.,2.95));
#13953=CARTESIAN_POINT('',(-0.71,-8.69499227394621E-17,2.95));
#13954=CARTESIAN_POINT('Origin',(0.,0.,2.95));
#13955=CARTESIAN_POINT('Origin',(0.,0.,3.6));
#13956=CARTESIAN_POINT('',(-0.71,-8.69499227394621E-17,4.4));
#13957=CARTESIAN_POINT('Origin',(0.,0.,4.4));
#13958=CARTESIAN_POINT('',(-0.71,-8.69499227394621E-17,3.6));
#13959=CARTESIAN_POINT('Origin',(0.,0.,3.6));
#13960=CARTESIAN_POINT('',(-2.2,-2.69422295812418E-16,4.4));
#13961=CARTESIAN_POINT('Origin',(0.,0.,4.4));
#13962=CARTESIAN_POINT('',(-2.2,-2.69422295812418E-16,3.6));
#13963=CARTESIAN_POINT('',(-2.2,-2.69422295812418E-16,3.6));
#13964=CARTESIAN_POINT('Origin',(0.,0.,3.6));
#13965=CARTESIAN_POINT('Origin',(0.,0.,4.4));
#13966=CARTESIAN_POINT('Origin',(0.,0.,3.6));
#13967=CARTESIAN_POINT('',(0.,0.,0.));
#13968=CARTESIAN_POINT('Origin',(5.5,3.1,2.));
#13969=CARTESIAN_POINT('',(5.1,3.1,2.));
#13970=CARTESIAN_POINT('',(5.1,3.1,5.));
#13971=CARTESIAN_POINT('',(5.1,3.1,2.));
#13972=CARTESIAN_POINT('',(5.5,3.5,2.));
#13973=CARTESIAN_POINT('Origin',(5.5,3.1,2.));
#13974=CARTESIAN_POINT('',(5.5,3.5,5.));
#13975=CARTESIAN_POINT('',(5.5,3.5,2.));
#13976=CARTESIAN_POINT('Origin',(5.5,3.1,5.));
#13977=CARTESIAN_POINT('Origin',(5.5,0.9,2.));
#13978=CARTESIAN_POINT('',(5.1,0.9,2.));
#13979=CARTESIAN_POINT('',(5.1,0.9,5.));
#13980=CARTESIAN_POINT('',(5.1,0.9,2.));
#13981=CARTESIAN_POINT('',(5.5,0.5,2.));
#13982=CARTESIAN_POINT('Origin',(5.5,0.9,2.));
#13983=CARTESIAN_POINT('',(5.5,0.5,5.));
#13984=CARTESIAN_POINT('',(5.5,0.5,2.));
#13985=CARTESIAN_POINT('Origin',(5.5,0.9,5.));
#13986=CARTESIAN_POINT('Origin',(5.5,2.,4.59));
#13987=CARTESIAN_POINT('',(5.3762058159686,1.89091287885364,4.59));
#13988=CARTESIAN_POINT('',(5.6237941840314,1.89091287885364,4.59));
#13989=CARTESIAN_POINT('',(4.9,1.89091287885364,4.59));
#13990=CARTESIAN_POINT('Origin',(5.5,2.,4.59));
#13991=CARTESIAN_POINT('Origin',(5.5,2.,4.59));
#13992=CARTESIAN_POINT('',(5.3762058159686,2.10908712114636,4.59));
#13993=CARTESIAN_POINT('',(5.335,2.,4.6));
#13994=CARTESIAN_POINT('Ctrl Pts',(5.3762058159686,2.10908712114636,4.59));
#13995=CARTESIAN_POINT('Ctrl Pts',(5.36460086481047,2.09591759715261,4.59243495840567));
#13996=CARTESIAN_POINT('Ctrl Pts',(5.35465435634175,2.08022344943772,4.59485638705045));
#13997=CARTESIAN_POINT('Ctrl Pts',(5.33918513536598,2.04298016596019,4.59880705606552));
#13998=CARTESIAN_POINT('Ctrl Pts',(5.335,2.02083185350888,4.6));
#13999=CARTESIAN_POINT('Ctrl Pts',(5.335,2.,4.6));
#14000=CARTESIAN_POINT('',(5.6237941840314,2.10908712114636,4.59));
#14001=CARTESIAN_POINT('Origin',(5.5,2.,4.59));
#14002=CARTESIAN_POINT('',(5.665,2.,4.6));
#14003=CARTESIAN_POINT('Ctrl Pts',(5.665,2.,4.6));
#14004=CARTESIAN_POINT('Ctrl Pts',(5.665,2.02083185350888,4.6));
#14005=CARTESIAN_POINT('Ctrl Pts',(5.66081486463402,2.04298016596019,4.59880705606552));
#14006=CARTESIAN_POINT('Ctrl Pts',(5.64534564365825,2.08022344943772,4.59485638705045));
#14007=CARTESIAN_POINT('Ctrl Pts',(5.63539913518953,2.09591759715261,4.59243495840567));
#14008=CARTESIAN_POINT('Ctrl Pts',(5.6237941840314,2.10908712114636,4.59));
#14009=CARTESIAN_POINT('Ctrl Pts',(5.6237941840314,1.89091287885364,4.59));
#14010=CARTESIAN_POINT('Ctrl Pts',(5.63539913518953,1.90408240284739,4.59243495840567));
#14011=CARTESIAN_POINT('Ctrl Pts',(5.64534564365825,1.91977655056228,4.59485638705045));
#14012=CARTESIAN_POINT('Ctrl Pts',(5.66081486463402,1.95701983403981,4.59880705606552));
#14013=CARTESIAN_POINT('Ctrl Pts',(5.665,1.97916814649112,4.6));
#14014=CARTESIAN_POINT('Ctrl Pts',(5.665,2.,4.6));
#14015=CARTESIAN_POINT('Ctrl Pts',(5.335,2.,4.6));
#14016=CARTESIAN_POINT('Ctrl Pts',(5.335,1.97916814649112,4.6));
#14017=CARTESIAN_POINT('Ctrl Pts',(5.33918513536598,1.95701983403981,4.59880705606552));
#14018=CARTESIAN_POINT('Ctrl Pts',(5.35465435634175,1.91977655056228,4.59485638705045));
#14019=CARTESIAN_POINT('Ctrl Pts',(5.36460086481047,1.90408240284739,4.59243495840567));
#14020=CARTESIAN_POINT('Ctrl Pts',(5.3762058159686,1.89091287885364,4.59));
#14021=CARTESIAN_POINT('',(5.335,2.,5.));
#14022=CARTESIAN_POINT('',(5.335,2.,4.59));
#14023=CARTESIAN_POINT('Origin',(5.5,2.,5.));
#14024=CARTESIAN_POINT('Origin',(5.5,2.,4.59));
#14025=CARTESIAN_POINT('',(4.9,2.10908712114636,4.59));
#14026=CARTESIAN_POINT('Origin',(5.5,0.9,2.));
#14027=CARTESIAN_POINT('Origin',(5.5,0.9,5.));
#14028=CARTESIAN_POINT('',(5.5,0.5,2.));
#14029=CARTESIAN_POINT('Origin',(5.5,0.9,2.));
#14030=CARTESIAN_POINT('Origin',(5.5,0.9,2.));
#14031=CARTESIAN_POINT('',(5.275,0.9,2.));
#14032=CARTESIAN_POINT('Origin',(5.5,0.9,2.));
#14033=CARTESIAN_POINT('Origin',(5.5,3.1,2.));
#14034=CARTESIAN_POINT('Origin',(5.5,3.1,5.));
#14035=CARTESIAN_POINT('',(5.5,3.5,2.));
#14036=CARTESIAN_POINT('Origin',(5.5,3.1,2.));
#14037=CARTESIAN_POINT('Origin',(5.5,3.1,2.));
#14038=CARTESIAN_POINT('',(5.275,3.1,2.));
#14039=CARTESIAN_POINT('Origin',(5.5,3.1,2.));
#14040=CARTESIAN_POINT('Origin',(5.5,2.,5.));
#14041=CARTESIAN_POINT('',(5.,3.5,5.));
#14042=CARTESIAN_POINT('',(5.,0.5,5.));
#14043=CARTESIAN_POINT('',(5.,3.5,5.));
#14044=CARTESIAN_POINT('',(5.,0.5,5.));
#14045=CARTESIAN_POINT('',(6.,0.5,5.));
#14046=CARTESIAN_POINT('',(5.,0.5,5.));
#14047=CARTESIAN_POINT('',(6.,3.5,5.));
#14048=CARTESIAN_POINT('',(6.,0.5,5.));
#14049=CARTESIAN_POINT('',(6.,3.5,5.));
#14050=CARTESIAN_POINT('',(6.,3.5,5.));
#14051=CARTESIAN_POINT('Origin',(5.5,0.9,0.9));
#14052=CARTESIAN_POINT('',(5.275,0.9,1.));
#14053=CARTESIAN_POINT('Origin',(5.5,0.9,1.));
#14054=CARTESIAN_POINT('',(5.275,0.9,0.9));
#14055=CARTESIAN_POINT('Origin',(5.5,3.1,0.9));
#14056=CARTESIAN_POINT('',(5.275,3.1,1.));
#14057=CARTESIAN_POINT('Origin',(5.5,3.1,1.));
#14058=CARTESIAN_POINT('',(5.275,3.1,0.9));
#14059=CARTESIAN_POINT('Origin',(4.9,2.,4.));
#14060=CARTESIAN_POINT('',(5.,2.,4.6));
#14061=CARTESIAN_POINT('Origin',(5.,2.,4.));
#14062=CARTESIAN_POINT('',(4.9,2.,4.6));
#14063=CARTESIAN_POINT('',(6.,2.,4.6));
#14064=CARTESIAN_POINT('',(4.9,2.,4.6));
#14065=CARTESIAN_POINT('Origin',(6.,2.,4.));
#14066=CARTESIAN_POINT('Origin',(6.,3.5,1.));
#14067=CARTESIAN_POINT('',(6.,3.5,1.));
#14068=CARTESIAN_POINT('',(5.,3.5,1.));
#14069=CARTESIAN_POINT('',(6.,3.5,1.));
#14070=CARTESIAN_POINT('',(5.,3.5,1.));
#14071=CARTESIAN_POINT('',(6.,3.5,1.));
#14072=CARTESIAN_POINT('Origin',(6.,0.5,1.));
#14073=CARTESIAN_POINT('',(6.,0.5,1.));
#14074=CARTESIAN_POINT('',(6.,0.5,1.));
#14075=CARTESIAN_POINT('',(6.,0.5,1.));
#14076=CARTESIAN_POINT('Origin',(5.,0.5,1.));
#14077=CARTESIAN_POINT('',(5.,0.5,1.));
#14078=CARTESIAN_POINT('',(5.,0.5,1.));
#14079=CARTESIAN_POINT('',(5.,0.5,1.));
#14080=CARTESIAN_POINT('Origin',(5.,3.5,1.));
#14081=CARTESIAN_POINT('',(5.,3.5,1.));
#14082=CARTESIAN_POINT('Origin',(5.5,2.,1.));
#14083=CARTESIAN_POINT('',(0.,0.,0.));
#14084=CARTESIAN_POINT('Origin',(15.5,3.1,2.));
#14085=CARTESIAN_POINT('',(15.1,3.1,2.));
#14086=CARTESIAN_POINT('',(15.1,3.1,5.));
#14087=CARTESIAN_POINT('',(15.1,3.1,2.));
#14088=CARTESIAN_POINT('',(15.5,3.5,2.));
#14089=CARTESIAN_POINT('Origin',(15.5,3.1,2.));
#14090=CARTESIAN_POINT('',(15.5,3.5,5.));
#14091=CARTESIAN_POINT('',(15.5,3.5,2.));
#14092=CARTESIAN_POINT('Origin',(15.5,3.1,5.));
#14093=CARTESIAN_POINT('Origin',(15.5,0.9,2.));
#14094=CARTESIAN_POINT('',(15.1,0.9,2.));
#14095=CARTESIAN_POINT('',(15.1,0.9,5.));
#14096=CARTESIAN_POINT('',(15.1,0.9,2.));
#14097=CARTESIAN_POINT('',(15.5,0.5,2.));
#14098=CARTESIAN_POINT('Origin',(15.5,0.9,2.));
#14099=CARTESIAN_POINT('',(15.5,0.5,5.));
#14100=CARTESIAN_POINT('',(15.5,0.5,2.));
#14101=CARTESIAN_POINT('Origin',(15.5,0.9,5.));
#14102=CARTESIAN_POINT('Origin',(15.5,2.,4.59));
#14103=CARTESIAN_POINT('',(15.3762058159686,1.89091287885364,4.59));
#14104=CARTESIAN_POINT('',(15.6237941840314,1.89091287885364,4.59));
#14105=CARTESIAN_POINT('',(14.9,1.89091287885364,4.59));
#14106=CARTESIAN_POINT('Origin',(15.5,2.,4.59));
#14107=CARTESIAN_POINT('Origin',(15.5,2.,4.59));
#14108=CARTESIAN_POINT('',(15.3762058159686,2.10908712114636,4.59));
#14109=CARTESIAN_POINT('',(15.335,2.,4.6));
#14110=CARTESIAN_POINT('Ctrl Pts',(15.3762058159686,2.10908712114636,4.59));
#14111=CARTESIAN_POINT('Ctrl Pts',(15.3646008648105,2.09591759715261,4.59243495840567));
#14112=CARTESIAN_POINT('Ctrl Pts',(15.3546543563418,2.08022344943772,4.59485638705045));
#14113=CARTESIAN_POINT('Ctrl Pts',(15.339185135366,2.04298016596019,4.59880705606552));
#14114=CARTESIAN_POINT('Ctrl Pts',(15.335,2.02083185350888,4.6));
#14115=CARTESIAN_POINT('Ctrl Pts',(15.335,2.,4.6));
#14116=CARTESIAN_POINT('',(15.6237941840314,2.10908712114636,4.59));
#14117=CARTESIAN_POINT('Origin',(15.5,2.,4.59));
#14118=CARTESIAN_POINT('',(15.665,2.,4.6));
#14119=CARTESIAN_POINT('Ctrl Pts',(15.665,2.,4.6));
#14120=CARTESIAN_POINT('Ctrl Pts',(15.665,2.02083185350888,4.6));
#14121=CARTESIAN_POINT('Ctrl Pts',(15.660814864634,2.04298016596019,4.59880705606552));
#14122=CARTESIAN_POINT('Ctrl Pts',(15.6453456436582,2.08022344943772,4.59485638705045));
#14123=CARTESIAN_POINT('Ctrl Pts',(15.6353991351895,2.09591759715261,4.59243495840567));
#14124=CARTESIAN_POINT('Ctrl Pts',(15.6237941840314,2.10908712114636,4.59));
#14125=CARTESIAN_POINT('Ctrl Pts',(15.6237941840314,1.89091287885364,4.59));
#14126=CARTESIAN_POINT('Ctrl Pts',(15.6353991351895,1.90408240284739,4.59243495840567));
#14127=CARTESIAN_POINT('Ctrl Pts',(15.6453456436582,1.91977655056228,4.59485638705045));
#14128=CARTESIAN_POINT('Ctrl Pts',(15.660814864634,1.95701983403981,4.59880705606552));
#14129=CARTESIAN_POINT('Ctrl Pts',(15.665,1.97916814649112,4.6));
#14130=CARTESIAN_POINT('Ctrl Pts',(15.665,2.,4.6));
#14131=CARTESIAN_POINT('Ctrl Pts',(15.335,2.,4.6));
#14132=CARTESIAN_POINT('Ctrl Pts',(15.335,1.97916814649112,4.6));
#14133=CARTESIAN_POINT('Ctrl Pts',(15.339185135366,1.95701983403981,4.59880705606552));
#14134=CARTESIAN_POINT('Ctrl Pts',(15.3546543563418,1.91977655056228,4.59485638705045));
#14135=CARTESIAN_POINT('Ctrl Pts',(15.3646008648105,1.90408240284739,4.59243495840567));
#14136=CARTESIAN_POINT('Ctrl Pts',(15.3762058159686,1.89091287885364,4.59));
#14137=CARTESIAN_POINT('',(15.335,2.,5.));
#14138=CARTESIAN_POINT('',(15.335,2.,4.59));
#14139=CARTESIAN_POINT('Origin',(15.5,2.,5.));
#14140=CARTESIAN_POINT('Origin',(15.5,2.,4.59));
#14141=CARTESIAN_POINT('',(14.9,2.10908712114636,4.59));
#14142=CARTESIAN_POINT('Origin',(15.5,0.9,2.));
#14143=CARTESIAN_POINT('Origin',(15.5,0.9,5.));
#14144=CARTESIAN_POINT('',(15.5,0.5,2.));
#14145=CARTESIAN_POINT('Origin',(15.5,0.9,2.));
#14146=CARTESIAN_POINT('Origin',(15.5,0.9,2.));
#14147=CARTESIAN_POINT('',(15.275,0.9,2.));
#14148=CARTESIAN_POINT('Origin',(15.5,0.9,2.));
#14149=CARTESIAN_POINT('Origin',(15.5,3.1,2.));
#14150=CARTESIAN_POINT('Origin',(15.5,3.1,5.));
#14151=CARTESIAN_POINT('',(15.5,3.5,2.));
#14152=CARTESIAN_POINT('Origin',(15.5,3.1,2.));
#14153=CARTESIAN_POINT('Origin',(15.5,3.1,2.));
#14154=CARTESIAN_POINT('',(15.275,3.1,2.));
#14155=CARTESIAN_POINT('Origin',(15.5,3.1,2.));
#14156=CARTESIAN_POINT('Origin',(15.5,2.,5.));
#14157=CARTESIAN_POINT('',(15.,3.5,5.));
#14158=CARTESIAN_POINT('',(15.,0.5,5.));
#14159=CARTESIAN_POINT('',(15.,3.5,5.));
#14160=CARTESIAN_POINT('',(15.,0.5,5.));
#14161=CARTESIAN_POINT('',(16.,0.5,5.));
#14162=CARTESIAN_POINT('',(15.,0.5,5.));
#14163=CARTESIAN_POINT('',(16.,3.5,5.));
#14164=CARTESIAN_POINT('',(16.,0.5,5.));
#14165=CARTESIAN_POINT('',(16.,3.5,5.));
#14166=CARTESIAN_POINT('',(16.,3.5,5.));
#14167=CARTESIAN_POINT('Origin',(15.5,0.9,0.9));
#14168=CARTESIAN_POINT('',(15.275,0.9,1.));
#14169=CARTESIAN_POINT('Origin',(15.5,0.9,1.));
#14170=CARTESIAN_POINT('',(15.275,0.9,0.9));
#14171=CARTESIAN_POINT('Origin',(15.5,3.1,0.9));
#14172=CARTESIAN_POINT('',(15.275,3.1,1.));
#14173=CARTESIAN_POINT('Origin',(15.5,3.1,1.));
#14174=CARTESIAN_POINT('',(15.275,3.1,0.9));
#14175=CARTESIAN_POINT('Origin',(14.9,2.,4.));
#14176=CARTESIAN_POINT('',(15.,2.,4.6));
#14177=CARTESIAN_POINT('Origin',(15.,2.,4.));
#14178=CARTESIAN_POINT('',(14.9,2.,4.6));
#14179=CARTESIAN_POINT('',(16.,2.,4.6));
#14180=CARTESIAN_POINT('',(14.9,2.,4.6));
#14181=CARTESIAN_POINT('Origin',(16.,2.,4.));
#14182=CARTESIAN_POINT('Origin',(16.,3.5,1.));
#14183=CARTESIAN_POINT('',(16.,3.5,1.));
#14184=CARTESIAN_POINT('',(15.,3.5,1.));
#14185=CARTESIAN_POINT('',(16.,3.5,1.));
#14186=CARTESIAN_POINT('',(15.,3.5,1.));
#14187=CARTESIAN_POINT('',(16.,3.5,1.));
#14188=CARTESIAN_POINT('Origin',(16.,0.5,1.));
#14189=CARTESIAN_POINT('',(16.,0.5,1.));
#14190=CARTESIAN_POINT('',(16.,0.5,1.));
#14191=CARTESIAN_POINT('',(16.,0.5,1.));
#14192=CARTESIAN_POINT('Origin',(15.,0.5,1.));
#14193=CARTESIAN_POINT('',(15.,0.5,1.));
#14194=CARTESIAN_POINT('',(15.,0.5,1.));
#14195=CARTESIAN_POINT('',(15.,0.5,1.));
#14196=CARTESIAN_POINT('Origin',(15.,3.5,1.));
#14197=CARTESIAN_POINT('',(15.,3.5,1.));
#14198=CARTESIAN_POINT('Origin',(15.5,2.,1.));
#14199=CARTESIAN_POINT('',(0.,0.,0.));
#14200=CARTESIAN_POINT('Origin',(5.1,7.5,2.));
#14201=CARTESIAN_POINT('',(4.7,7.5,2.));
#14202=CARTESIAN_POINT('',(4.7,7.5,5.));
#14203=CARTESIAN_POINT('',(4.7,7.5,2.));
#14204=CARTESIAN_POINT('',(5.5,7.5,2.));
#14205=CARTESIAN_POINT('Origin',(5.1,7.5,2.));
#14206=CARTESIAN_POINT('',(5.5,7.5,5.));
#14207=CARTESIAN_POINT('',(5.5,7.5,2.));
#14208=CARTESIAN_POINT('Origin',(5.1,7.5,5.));
#14209=CARTESIAN_POINT('Origin',(4.,7.5,4.59));
#14210=CARTESIAN_POINT('',(4.10908712114636,7.3762058159686,4.59));
#14211=CARTESIAN_POINT('',(4.10908712114636,7.6237941840314,4.59));
#14212=CARTESIAN_POINT('',(4.10908712114636,6.9,4.59));
#14213=CARTESIAN_POINT('Origin',(4.,7.5,4.59));
#14214=CARTESIAN_POINT('Origin',(4.,7.5,4.59));
#14215=CARTESIAN_POINT('',(3.89091287885364,7.3762058159686,4.59));
#14216=CARTESIAN_POINT('Ctrl Pts',(3.89091287885364,7.3762058159686,4.59));
#14217=CARTESIAN_POINT('Ctrl Pts',(3.90408240284739,7.36460086481046,4.59243495840567));
#14218=CARTESIAN_POINT('Ctrl Pts',(3.91977655056228,7.35465435634175,4.59485638705045));
#14219=CARTESIAN_POINT('Ctrl Pts',(3.95701983403981,7.33918513536598,4.59880705606552));
#14220=CARTESIAN_POINT('Ctrl Pts',(3.97916814649112,7.335,4.6));
#14221=CARTESIAN_POINT('Ctrl Pts',(4.02083185350888,7.335,4.6));
#14222=CARTESIAN_POINT('Ctrl Pts',(4.04298016596019,7.33918513536598,4.59880705606552));
#14223=CARTESIAN_POINT('Ctrl Pts',(4.08022344943772,7.35465435634175,4.59485638705045));
#14224=CARTESIAN_POINT('Ctrl Pts',(4.09591759715261,7.36460086481046,4.59243495840567));
#14225=CARTESIAN_POINT('Ctrl Pts',(4.10908712114636,7.3762058159686,4.59));
#14226=CARTESIAN_POINT('',(3.835,7.5,4.59));
#14227=CARTESIAN_POINT('Origin',(4.,7.5,4.59));
#14228=CARTESIAN_POINT('',(3.835,7.5,5.));
#14229=CARTESIAN_POINT('',(3.835,7.5,4.59));
#14230=CARTESIAN_POINT('Origin',(4.,7.5,5.));
#14231=CARTESIAN_POINT('',(3.89091287885364,7.6237941840314,4.59));
#14232=CARTESIAN_POINT('Origin',(4.,7.5,4.59));
#14233=CARTESIAN_POINT('Ctrl Pts',(4.10908712114636,7.6237941840314,4.59));
#14234=CARTESIAN_POINT('Ctrl Pts',(4.09591759715261,7.63539913518953,4.59243495840567));
#14235=CARTESIAN_POINT('Ctrl Pts',(4.08022344943772,7.64534564365825,4.59485638705045));
#14236=CARTESIAN_POINT('Ctrl Pts',(4.04298016596019,7.66081486463402,4.59880705606552));
#14237=CARTESIAN_POINT('Ctrl Pts',(4.02083185350888,7.665,4.6));
#14238=CARTESIAN_POINT('Ctrl Pts',(3.97916814649112,7.665,4.6));
#14239=CARTESIAN_POINT('Ctrl Pts',(3.95701983403981,7.66081486463402,4.59880705606552));
#14240=CARTESIAN_POINT('Ctrl Pts',(3.91977655056228,7.64534564365825,4.59485638705045));
#14241=CARTESIAN_POINT('Ctrl Pts',(3.90408240284739,7.63539913518954,4.59243495840567));
#14242=CARTESIAN_POINT('Ctrl Pts',(3.89091287885364,7.6237941840314,4.59));
#14243=CARTESIAN_POINT('Origin',(4.,7.5,4.59));
#14244=CARTESIAN_POINT('',(3.89091287885364,6.9,4.59));
#14245=CARTESIAN_POINT('Origin',(2.9,7.5,2.));
#14246=CARTESIAN_POINT('',(2.5,7.5,2.));
#14247=CARTESIAN_POINT('Origin',(2.9,7.5,2.));
#14248=CARTESIAN_POINT('',(2.5,7.5,5.));
#14249=CARTESIAN_POINT('',(2.5,7.5,2.));
#14250=CARTESIAN_POINT('Origin',(2.9,7.5,5.));
#14251=CARTESIAN_POINT('',(2.5,7.5,2.));
#14252=CARTESIAN_POINT('Origin',(2.9,7.5,2.));
#14253=CARTESIAN_POINT('',(2.675,7.5,2.));
#14254=CARTESIAN_POINT('Origin',(2.9,7.5,2.));
#14255=CARTESIAN_POINT('Origin',(5.1,7.5,2.));
#14256=CARTESIAN_POINT('Origin',(5.1,7.5,5.));
#14257=CARTESIAN_POINT('',(5.5,7.5,2.));
#14258=CARTESIAN_POINT('Origin',(5.1,7.5,2.));
#14259=CARTESIAN_POINT('Origin',(5.1,7.5,2.));
#14260=CARTESIAN_POINT('',(4.875,7.5,2.));
#14261=CARTESIAN_POINT('Origin',(5.1,7.5,2.));
#14262=CARTESIAN_POINT('Origin',(4.,7.5,5.));
#14263=CARTESIAN_POINT('',(2.5,8.,5.));
#14264=CARTESIAN_POINT('',(2.5,8.,5.));
#14265=CARTESIAN_POINT('',(2.5,7.,5.));
#14266=CARTESIAN_POINT('',(2.5,8.,5.));
#14267=CARTESIAN_POINT('',(5.5,7.,5.));
#14268=CARTESIAN_POINT('',(2.5,7.,5.));
#14269=CARTESIAN_POINT('',(5.5,7.,5.));
#14270=CARTESIAN_POINT('',(5.5,8.,5.));
#14271=CARTESIAN_POINT('',(5.5,7.,5.));
#14272=CARTESIAN_POINT('',(5.5,8.,5.));
#14273=CARTESIAN_POINT('Origin',(2.9,7.5,0.9));
#14274=CARTESIAN_POINT('',(2.675,7.5,1.));
#14275=CARTESIAN_POINT('Origin',(2.9,7.5,1.));
#14276=CARTESIAN_POINT('',(2.675,7.5,0.9));
#14277=CARTESIAN_POINT('Origin',(5.1,7.5,0.9));
#14278=CARTESIAN_POINT('',(4.875,7.5,1.));
#14279=CARTESIAN_POINT('Origin',(5.1,7.5,1.));
#14280=CARTESIAN_POINT('',(4.875,7.5,0.9));
#14281=CARTESIAN_POINT('Origin',(4.,6.9,4.));
#14282=CARTESIAN_POINT('',(3.4,7.,4.));
#14283=CARTESIAN_POINT('Origin',(4.,7.,4.));
#14284=CARTESIAN_POINT('',(3.4,8.,4.));
#14285=CARTESIAN_POINT('',(3.4,6.9,4.));
#14286=CARTESIAN_POINT('Origin',(4.,8.,4.));
#14287=CARTESIAN_POINT('Origin',(5.5,8.,1.));
#14288=CARTESIAN_POINT('',(5.5,8.,1.));
#14289=CARTESIAN_POINT('',(2.5,8.,1.));
#14290=CARTESIAN_POINT('',(5.5,8.,1.));
#14291=CARTESIAN_POINT('',(2.5,8.,1.));
#14292=CARTESIAN_POINT('',(5.5,8.,1.));
#14293=CARTESIAN_POINT('Origin',(5.5,7.,1.));
#14294=CARTESIAN_POINT('',(5.5,7.,1.));
#14295=CARTESIAN_POINT('',(5.5,7.,1.));
#14296=CARTESIAN_POINT('',(5.5,7.,1.));
#14297=CARTESIAN_POINT('Origin',(2.5,7.,1.));
#14298=CARTESIAN_POINT('',(2.5,7.,1.));
#14299=CARTESIAN_POINT('',(2.5,7.,1.));
#14300=CARTESIAN_POINT('',(2.5,7.,1.));
#14301=CARTESIAN_POINT('Origin',(2.5,8.,1.));
#14302=CARTESIAN_POINT('',(2.5,8.,1.));
#14303=CARTESIAN_POINT('Origin',(4.,7.5,1.));
#14304=CARTESIAN_POINT('',(0.,0.,0.));
#14305=CARTESIAN_POINT('Origin',(5.1,17.5,2.));
#14306=CARTESIAN_POINT('',(4.7,17.5,2.));
#14307=CARTESIAN_POINT('',(4.7,17.5,5.));
#14308=CARTESIAN_POINT('',(4.7,17.5,2.));
#14309=CARTESIAN_POINT('',(5.5,17.5,2.));
#14310=CARTESIAN_POINT('Origin',(5.1,17.5,2.));
#14311=CARTESIAN_POINT('',(5.5,17.5,5.));
#14312=CARTESIAN_POINT('',(5.5,17.5,2.));
#14313=CARTESIAN_POINT('Origin',(5.1,17.5,5.));
#14314=CARTESIAN_POINT('Origin',(4.,17.5,4.59));
#14315=CARTESIAN_POINT('',(4.10908712114636,17.3762058159686,4.59));
#14316=CARTESIAN_POINT('',(4.10908712114636,17.6237941840314,4.59));
#14317=CARTESIAN_POINT('',(4.10908712114636,16.9,4.59));
#14318=CARTESIAN_POINT('Origin',(4.,17.5,4.59));
#14319=CARTESIAN_POINT('Origin',(4.,17.5,4.59));
#14320=CARTESIAN_POINT('',(3.89091287885364,17.3762058159686,4.59));
#14321=CARTESIAN_POINT('Ctrl Pts',(3.89091287885364,17.3762058159686,4.59));
#14322=CARTESIAN_POINT('Ctrl Pts',(3.90408240284739,17.3646008648105,4.59243495840567));
#14323=CARTESIAN_POINT('Ctrl Pts',(3.91977655056228,17.3546543563418,4.59485638705045));
#14324=CARTESIAN_POINT('Ctrl Pts',(3.95701983403981,17.339185135366,4.59880705606552));
#14325=CARTESIAN_POINT('Ctrl Pts',(3.97916814649112,17.335,4.6));
#14326=CARTESIAN_POINT('Ctrl Pts',(4.02083185350888,17.335,4.6));
#14327=CARTESIAN_POINT('Ctrl Pts',(4.04298016596019,17.339185135366,4.59880705606552));
#14328=CARTESIAN_POINT('Ctrl Pts',(4.08022344943772,17.3546543563418,4.59485638705045));
#14329=CARTESIAN_POINT('Ctrl Pts',(4.09591759715261,17.3646008648105,4.59243495840567));
#14330=CARTESIAN_POINT('Ctrl Pts',(4.10908712114636,17.3762058159686,4.59));
#14331=CARTESIAN_POINT('',(3.835,17.5,4.59));
#14332=CARTESIAN_POINT('Origin',(4.,17.5,4.59));
#14333=CARTESIAN_POINT('',(3.835,17.5,5.));
#14334=CARTESIAN_POINT('',(3.835,17.5,4.59));
#14335=CARTESIAN_POINT('Origin',(4.,17.5,5.));
#14336=CARTESIAN_POINT('',(3.89091287885364,17.6237941840314,4.59));
#14337=CARTESIAN_POINT('Origin',(4.,17.5,4.59));
#14338=CARTESIAN_POINT('Ctrl Pts',(4.10908712114636,17.6237941840314,4.59));
#14339=CARTESIAN_POINT('Ctrl Pts',(4.09591759715261,17.6353991351895,4.59243495840567));
#14340=CARTESIAN_POINT('Ctrl Pts',(4.08022344943772,17.6453456436582,4.59485638705045));
#14341=CARTESIAN_POINT('Ctrl Pts',(4.04298016596019,17.660814864634,4.59880705606552));
#14342=CARTESIAN_POINT('Ctrl Pts',(4.02083185350888,17.665,4.6));
#14343=CARTESIAN_POINT('Ctrl Pts',(3.97916814649112,17.665,4.6));
#14344=CARTESIAN_POINT('Ctrl Pts',(3.95701983403981,17.660814864634,4.59880705606552));
#14345=CARTESIAN_POINT('Ctrl Pts',(3.91977655056228,17.6453456436582,4.59485638705045));
#14346=CARTESIAN_POINT('Ctrl Pts',(3.90408240284739,17.6353991351895,4.59243495840567));
#14347=CARTESIAN_POINT('Ctrl Pts',(3.89091287885364,17.6237941840314,4.59));
#14348=CARTESIAN_POINT('Origin',(4.,17.5,4.59));
#14349=CARTESIAN_POINT('',(3.89091287885364,16.9,4.59));
#14350=CARTESIAN_POINT('Origin',(2.9,17.5,2.));
#14351=CARTESIAN_POINT('',(2.5,17.5,2.));
#14352=CARTESIAN_POINT('Origin',(2.9,17.5,2.));
#14353=CARTESIAN_POINT('',(2.5,17.5,5.));
#14354=CARTESIAN_POINT('',(2.5,17.5,2.));
#14355=CARTESIAN_POINT('Origin',(2.9,17.5,5.));
#14356=CARTESIAN_POINT('',(2.5,17.5,2.));
#14357=CARTESIAN_POINT('Origin',(2.9,17.5,2.));
#14358=CARTESIAN_POINT('',(2.675,17.5,2.));
#14359=CARTESIAN_POINT('Origin',(2.9,17.5,2.));
#14360=CARTESIAN_POINT('Origin',(5.1,17.5,2.));
#14361=CARTESIAN_POINT('Origin',(5.1,17.5,5.));
#14362=CARTESIAN_POINT('',(5.5,17.5,2.));
#14363=CARTESIAN_POINT('Origin',(5.1,17.5,2.));
#14364=CARTESIAN_POINT('Origin',(5.1,17.5,2.));
#14365=CARTESIAN_POINT('',(4.875,17.5,2.));
#14366=CARTESIAN_POINT('Origin',(5.1,17.5,2.));
#14367=CARTESIAN_POINT('Origin',(4.,17.5,5.));
#14368=CARTESIAN_POINT('',(2.5,18.,5.));
#14369=CARTESIAN_POINT('',(2.5,18.,5.));
#14370=CARTESIAN_POINT('',(2.5,17.,5.));
#14371=CARTESIAN_POINT('',(2.5,18.,5.));
#14372=CARTESIAN_POINT('',(5.5,17.,5.));
#14373=CARTESIAN_POINT('',(2.5,17.,5.));
#14374=CARTESIAN_POINT('',(5.5,17.,5.));
#14375=CARTESIAN_POINT('',(5.5,18.,5.));
#14376=CARTESIAN_POINT('',(5.5,17.,5.));
#14377=CARTESIAN_POINT('',(5.5,18.,5.));
#14378=CARTESIAN_POINT('Origin',(2.9,17.5,0.9));
#14379=CARTESIAN_POINT('',(2.675,17.5,1.));
#14380=CARTESIAN_POINT('Origin',(2.9,17.5,1.));
#14381=CARTESIAN_POINT('',(2.675,17.5,0.9));
#14382=CARTESIAN_POINT('Origin',(5.1,17.5,0.9));
#14383=CARTESIAN_POINT('',(4.875,17.5,1.));
#14384=CARTESIAN_POINT('Origin',(5.1,17.5,1.));
#14385=CARTESIAN_POINT('',(4.875,17.5,0.9));
#14386=CARTESIAN_POINT('Origin',(4.,16.9,4.));
#14387=CARTESIAN_POINT('',(3.4,17.,4.));
#14388=CARTESIAN_POINT('Origin',(4.,17.,4.));
#14389=CARTESIAN_POINT('',(3.4,18.,4.));
#14390=CARTESIAN_POINT('',(3.4,16.9,4.));
#14391=CARTESIAN_POINT('Origin',(4.,18.,4.));
#14392=CARTESIAN_POINT('Origin',(5.5,18.,1.));
#14393=CARTESIAN_POINT('',(5.5,18.,1.));
#14394=CARTESIAN_POINT('',(2.5,18.,1.));
#14395=CARTESIAN_POINT('',(5.5,18.,1.));
#14396=CARTESIAN_POINT('',(2.5,18.,1.));
#14397=CARTESIAN_POINT('',(5.5,18.,1.));
#14398=CARTESIAN_POINT('Origin',(5.5,17.,1.));
#14399=CARTESIAN_POINT('',(5.5,17.,1.));
#14400=CARTESIAN_POINT('',(5.5,17.,1.));
#14401=CARTESIAN_POINT('',(5.5,17.,1.));
#14402=CARTESIAN_POINT('Origin',(2.5,17.,1.));
#14403=CARTESIAN_POINT('',(2.5,17.,1.));
#14404=CARTESIAN_POINT('',(2.5,17.,1.));
#14405=CARTESIAN_POINT('',(2.5,17.,1.));
#14406=CARTESIAN_POINT('Origin',(2.5,18.,1.));
#14407=CARTESIAN_POINT('',(2.5,18.,1.));
#14408=CARTESIAN_POINT('Origin',(4.,17.5,1.));
#14409=CARTESIAN_POINT('',(0.,0.,0.));
#14410=CARTESIAN_POINT('Origin',(0.115470053837925,-0.5,-0.2));
#14411=CARTESIAN_POINT('',(0.23094010767585,-0.5,0.));
#14412=CARTESIAN_POINT('',(0.115470053837925,-0.5,-0.2));
#14413=CARTESIAN_POINT('',(0.23094010767585,-0.5,0.));
#14414=CARTESIAN_POINT('',(0.115470053837925,-0.8,-0.2));
#14415=CARTESIAN_POINT('',(0.115470053837925,-0.5,-0.2));
#14416=CARTESIAN_POINT('',(0.23094010767585,-0.8,0.));
#14417=CARTESIAN_POINT('',(0.23094010767585,-0.8,0.));
#14418=CARTESIAN_POINT('',(0.23094010767585,-0.5,0.));
#14419=CARTESIAN_POINT('Origin',(-0.115470053837925,-0.5,-0.2));
#14420=CARTESIAN_POINT('',(-0.115470053837925,-0.5,-0.2));
#14421=CARTESIAN_POINT('',(0.115470053837925,-0.5,-0.2));
#14422=CARTESIAN_POINT('',(-0.115470053837925,-0.8,-0.2));
#14423=CARTESIAN_POINT('',(-0.115470053837925,-0.5,-0.2));
#14424=CARTESIAN_POINT('',(0.115470053837925,-0.8,-0.2));
#14425=CARTESIAN_POINT('Origin',(-0.23094010767585,-0.5,-2.77555756156289E-17));
#14426=CARTESIAN_POINT('',(-0.23094010767585,-0.5,-2.82820063659975E-17));
#14427=CARTESIAN_POINT('',(-0.115470053837925,-0.5,-0.2));
#14428=CARTESIAN_POINT('',(-0.23094010767585,-0.8,-2.77555756156289E-17));
#14429=CARTESIAN_POINT('',(-0.23094010767585,-0.5,-2.82820063659975E-17));
#14430=CARTESIAN_POINT('',(-0.115470053837925,-0.8,-0.2));
#14431=CARTESIAN_POINT('Origin',(-0.115470053837925,-0.5,0.2));
#14432=CARTESIAN_POINT('',(-0.115470053837925,-0.5,0.2));
#14433=CARTESIAN_POINT('',(-0.23094010767585,-0.5,-2.82820063659975E-17));
#14434=CARTESIAN_POINT('',(-0.115470053837925,-0.8,0.2));
#14435=CARTESIAN_POINT('',(-0.115470053837925,-0.5,0.2));
#14436=CARTESIAN_POINT('',(-0.23094010767585,-0.8,-2.82820063659975E-17));
#14437=CARTESIAN_POINT('Origin',(0.115470053837925,-0.5,0.2));
#14438=CARTESIAN_POINT('',(0.115470053837925,-0.5,0.2));
#14439=CARTESIAN_POINT('',(-0.115470053837925,-0.5,0.2));
#14440=CARTESIAN_POINT('',(0.115470053837925,-0.8,0.2));
#14441=CARTESIAN_POINT('',(0.115470053837925,-0.5,0.2));
#14442=CARTESIAN_POINT('',(-0.115470053837925,-0.8,0.2));
#14443=CARTESIAN_POINT('Origin',(0.23094010767585,-0.5,0.));
#14444=CARTESIAN_POINT('',(0.115470053837925,-0.5,0.2));
#14445=CARTESIAN_POINT('',(0.115470053837925,-0.8,0.2));
#14446=CARTESIAN_POINT('Origin',(0.,-0.5,0.));
#14447=CARTESIAN_POINT('Origin',(0.,-0.8,0.));
#14448=CARTESIAN_POINT('Origin',(0.,-1.4,0.));
#14449=CARTESIAN_POINT('',(-0.24505,-1.4,3.00099698131059E-17));
#14450=CARTESIAN_POINT('Origin',(0.,-1.4,0.));
#14451=CARTESIAN_POINT('Origin',(0.375,0.5,0.));
#14452=CARTESIAN_POINT('',(-0.375,0.5,-4.59242549680257E-17));
#14453=CARTESIAN_POINT('Origin',(0.,0.5,0.));
#14454=CARTESIAN_POINT('Origin',(0.,0.475,0.));
#14455=CARTESIAN_POINT('',(-0.425,0.45,-5.20474889637625E-17));
#14456=CARTESIAN_POINT('Origin',(0.,0.45,0.));
#14457=CARTESIAN_POINT('',(-0.4,0.475,-4.89858719658941E-17));
#14458=CARTESIAN_POINT('Origin',(0.,0.24,0.));
#14459=CARTESIAN_POINT('',(-0.425,0.0299999999999998,-5.20474889637625E-17));
#14460=CARTESIAN_POINT('Origin',(0.,0.0299999999999998,0.));
#14461=CARTESIAN_POINT('',(-0.425,0.24,-5.20474889637625E-17));
#14462=CARTESIAN_POINT('Origin',(0.,0.0150000000000001,0.));
#14463=CARTESIAN_POINT('',(-0.395,4.85722573273506E-17,-4.83735485663204E-17));
#14464=CARTESIAN_POINT('Origin',(0.,0.,0.));
#14465=CARTESIAN_POINT('',(-0.41,0.0150000000000001,-5.02105187650415E-17));
#14466=CARTESIAN_POINT('Origin',(0.27,0.,0.));
#14467=CARTESIAN_POINT('',(-0.27,0.,-3.30654635769785E-17));
#14468=CARTESIAN_POINT('Origin',(0.,0.,0.));
#14469=CARTESIAN_POINT('Origin',(0.,-0.02,0.));
#14470=CARTESIAN_POINT('',(-0.24505,-0.0498999999999999,3.00099698131059E-17));
#14471=CARTESIAN_POINT('Origin',(0.,-0.0498999999999999,0.));
#14472=CARTESIAN_POINT('',(-0.26,-0.02,-3.18408167778312E-17));
#14473=CARTESIAN_POINT('Origin',(0.,-0.995,0.));
#14474=CARTESIAN_POINT('',(-0.24505,-0.995,-3.00099698131059E-17));
#14475=CARTESIAN_POINT('',(0.,0.,0.));
#14476=CARTESIAN_POINT('',(0.,0.,0.));
#14477=CARTESIAN_POINT('Origin',(0.,0.,0.));
#14478=CARTESIAN_POINT('',(-0.976185,-0.246528389340863,-1.19548183562566E-16));
#14479=CARTESIAN_POINT('',(-1.19548183562566E-16,-0.246528389340863,0.976185));
#14480=CARTESIAN_POINT('Origin',(0.,-0.246528389340863,0.));
#14481=CARTESIAN_POINT('Origin',(0.,-0.246528389340863,0.));
#14482=CARTESIAN_POINT('',(-1.19548183562566E-16,0.246528389340863,0.976185));
#14483=CARTESIAN_POINT('Origin',(-1.22464679914735E-16,0.,1.));
#14484=CARTESIAN_POINT('',(-0.976185,0.246528389340863,1.19548183562566E-16));
#14485=CARTESIAN_POINT('Origin',(0.,0.246528389340863,0.));
#14486=CARTESIAN_POINT('Origin',(0.,0.246528389340863,0.));
#14487=CARTESIAN_POINT('Origin',(0.,0.,0.));
#14488=CARTESIAN_POINT('',(-0.976185,0.45,-1.19548183562566E-16));
#14489=CARTESIAN_POINT('',(-0.976185,0.,-1.19548183562566E-16));
#14490=CARTESIAN_POINT('Origin',(0.,0.45,0.));
#14491=CARTESIAN_POINT('Origin',(0.,0.,0.));
#14492=CARTESIAN_POINT('',(-0.5,-0.39,-6.12323399573677E-17));
#14493=CARTESIAN_POINT('Origin',(0.,-0.39,0.));
#14494=CARTESIAN_POINT('',(-0.5,0.39,-6.12323399573677E-17));
#14495=CARTESIAN_POINT('',(-0.5,0.,-6.12323399573677E-17));
#14496=CARTESIAN_POINT('Origin',(0.,0.39,0.));
#14497=CARTESIAN_POINT('Origin',(0.,0.42,0.));
#14498=CARTESIAN_POINT('',(-0.56,0.45,-6.85802207522518E-17));
#14499=CARTESIAN_POINT('',(-0.53,0.42,-6.49062803548097E-17));
#14500=CARTESIAN_POINT('Origin',(0.,0.45,0.));
#14501=CARTESIAN_POINT('Origin',(0.976185,0.45,0.));
#14502=CARTESIAN_POINT('Origin',(0.,0.,0.));
#14503=CARTESIAN_POINT('',(-0.976185,-0.45,-1.19548183562566E-16));
#14504=CARTESIAN_POINT('Origin',(0.,-0.45,0.));
#14505=CARTESIAN_POINT('',(-0.976185,0.,-1.19548183562566E-16));
#14506=CARTESIAN_POINT('Origin',(0.56,-0.45,0.));
#14507=CARTESIAN_POINT('',(-0.56,-0.45,-6.85802207522518E-17));
#14508=CARTESIAN_POINT('Origin',(0.,-0.45,0.));
#14509=CARTESIAN_POINT('Origin',(0.,-0.42,0.));
#14510=CARTESIAN_POINT('',(-0.53,-0.42,-6.49062803548097E-17));
#14511=CARTESIAN_POINT('',(0.,0.,0.));
#14512=CARTESIAN_POINT('Origin',(0.,0.,0.));
#14513=CARTESIAN_POINT('',(-1.023815,0.246528389340863,-1.25381176266905E-16));
#14514=CARTESIAN_POINT('',(-1.25381176266905E-16,0.246528389340863,1.023815));
#14515=CARTESIAN_POINT('Origin',(0.,0.246528389340863,0.));
#14516=CARTESIAN_POINT('Origin',(0.,0.246528389340863,0.));
#14517=CARTESIAN_POINT('',(-1.25381176266905E-16,-0.246528389340863,1.023815));
#14518=CARTESIAN_POINT('Origin',(-1.22464679914735E-16,0.,1.));
#14519=CARTESIAN_POINT('',(-1.023815,-0.246528389340863,1.25381176266905E-16));
#14520=CARTESIAN_POINT('Origin',(0.,-0.246528389340863,0.));
#14521=CARTESIAN_POINT('Origin',(0.,-0.246528389340863,0.));
#14522=CARTESIAN_POINT('Origin',(0.,0.,0.));
#14523=CARTESIAN_POINT('',(-1.023815,-0.45,-1.25381176266905E-16));
#14524=CARTESIAN_POINT('Origin',(0.,-0.45,0.));
#14525=CARTESIAN_POINT('',(-1.023815,0.,-1.25381176266905E-16));
#14526=CARTESIAN_POINT('Origin',(1.44,0.45,0.));
#14527=CARTESIAN_POINT('',(-1.44,0.45,-1.76349139077219E-16));
#14528=CARTESIAN_POINT('Origin',(0.,0.45,0.));
#14529=CARTESIAN_POINT('',(-1.023815,0.45,-1.25381176266905E-16));
#14530=CARTESIAN_POINT('Origin',(0.,0.45,0.));
#14531=CARTESIAN_POINT('Origin',(0.,0.42,0.));
#14532=CARTESIAN_POINT('',(-1.5,0.39,-1.83697019872103E-16));
#14533=CARTESIAN_POINT('Origin',(0.,0.39,0.));
#14534=CARTESIAN_POINT('',(-1.47,0.42,-1.80023079474661E-16));
#14535=CARTESIAN_POINT('Origin',(0.,0.,0.));
#14536=CARTESIAN_POINT('',(-1.5,-0.39,-1.83697019872103E-16));
#14537=CARTESIAN_POINT('Origin',(0.,-0.39,0.));
#14538=CARTESIAN_POINT('',(-1.5,0.,-1.83697019872103E-16));
#14539=CARTESIAN_POINT('Origin',(0.,-0.42,0.));
#14540=CARTESIAN_POINT('',(-1.44,-0.45,-1.76349139077219E-16));
#14541=CARTESIAN_POINT('Origin',(0.,-0.45,0.));
#14542=CARTESIAN_POINT('',(-1.47,-0.42,-1.80023079474661E-16));
#14543=CARTESIAN_POINT('Origin',(1.023815,-0.45,0.));
#14544=CARTESIAN_POINT('Origin',(0.,0.,0.));
#14545=CARTESIAN_POINT('',(-1.023815,0.,-1.25381176266905E-16));
#14546=CARTESIAN_POINT('',(0.,0.,0.));
#14547=CARTESIAN_POINT('Origin',(1.,0.,0.));
#14548=CARTESIAN_POINT('',(1.,-1.78583896120461E-33,0.23815));
#14549=CARTESIAN_POINT('',(1.,-1.78583896120461E-33,-0.23815));
#14550=CARTESIAN_POINT('Origin',(1.,0.,0.));
#14551=CARTESIAN_POINT('Origin',(0.707106781186548,0.,-0.707106781186547));
#14552=CARTESIAN_POINT('',(0.875504261126124,-1.78583896120461E-33,-0.538709301246971));
#14553=CARTESIAN_POINT('',(0.538709301246971,-1.78583896120461E-33,-0.875504261126124));
#14554=CARTESIAN_POINT('Origin',(0.707106781186548,0.,-0.707106781186547));
#14555=CARTESIAN_POINT('Origin',(6.12323399573677E-17,0.,-1.));
#14556=CARTESIAN_POINT('',(0.23815,-1.78583896120461E-33,-1.));
#14557=CARTESIAN_POINT('',(-0.23815,-1.78583896120461E-33,-1.));
#14558=CARTESIAN_POINT('Origin',(6.12323399573677E-17,0.,-1.));
#14559=CARTESIAN_POINT('Origin',(-0.707106781186547,0.,-0.707106781186548));
#14560=CARTESIAN_POINT('',(-0.538709301246971,-1.78583896120461E-33,-0.875504261126124));
#14561=CARTESIAN_POINT('',(-0.875504261126124,-1.78583896120461E-33,-0.538709301246971));
#14562=CARTESIAN_POINT('Origin',(-0.707106781186547,0.,-0.707106781186548));
#14563=CARTESIAN_POINT('Origin',(-1.,0.,-1.22464679914735E-16));
#14564=CARTESIAN_POINT('',(-1.,-1.78583896120461E-33,-0.23815));
#14565=CARTESIAN_POINT('',(-1.,-1.78583896120461E-33,0.23815));
#14566=CARTESIAN_POINT('Origin',(-1.,0.,-1.22464679914735E-16));
#14567=CARTESIAN_POINT('Origin',(-0.707106781186548,0.,0.707106781186547));
#14568=CARTESIAN_POINT('',(-0.875504261126124,-7.94881478324376E-33,0.538709301246971));
#14569=CARTESIAN_POINT('',(-0.538709301246971,4.37713686083455E-33,0.875504261126124));
#14570=CARTESIAN_POINT('Origin',(-0.707106781186548,0.,0.707106781186547));
#14571=CARTESIAN_POINT('Origin',(-1.83697019872103E-16,0.,1.));
#14572=CARTESIAN_POINT('',(-0.23815,-1.78583896120461E-33,1.));
#14573=CARTESIAN_POINT('',(0.23815,-1.78583896120461E-33,1.));
#14574=CARTESIAN_POINT('Origin',(-1.83697019872103E-16,0.,1.));
#14575=CARTESIAN_POINT('Origin',(0.707106781186547,0.,0.707106781186548));
#14576=CARTESIAN_POINT('',(0.538709301246971,-4.86732687222419E-33,0.875504261126124));
#14577=CARTESIAN_POINT('',(0.875504261126124,1.29564894981497E-33,0.538709301246971));
#14578=CARTESIAN_POINT('Origin',(0.707106781186547,0.,0.707106781186548));
#14579=CARTESIAN_POINT('',(0.,0.,0.));
#14580=CARTESIAN_POINT('Origin',(0.707106781186547,0.,0.707106781186548));
#14581=CARTESIAN_POINT('',(0.504455939115715,-0.04763,0.841298510752802));
#14582=CARTESIAN_POINT('',(0.841298510752802,-0.04763,0.504455939115715));
#14583=CARTESIAN_POINT('Ctrl Pts',(0.504455939115715,-0.04763,0.841298510752802));
#14584=CARTESIAN_POINT('Ctrl Pts',(0.508899795931835,-0.0740444353928835,
0.838633903678357));
#14585=CARTESIAN_POINT('Ctrl Pts',(0.517157748491652,-0.0999305678883309,
0.833661031856294));
#14586=CARTESIAN_POINT('Ctrl Pts',(0.537715343527944,-0.142345102874864,
0.820511285096538));
#14587=CARTESIAN_POINT('Ctrl Pts',(0.548874290046456,-0.159766064500479,
0.813159949759));
#14588=CARTESIAN_POINT('Ctrl Pts',(0.573915184558107,-0.190326085855194,
0.795684265985089));
#14589=CARTESIAN_POINT('Ctrl Pts',(0.587792702767295,-0.203463743702801,
0.78555112003688));
#14590=CARTESIAN_POINT('Ctrl Pts',(0.615966552324775,-0.224161999508995,
0.763642258217233));
#14591=CARTESIAN_POINT('Ctrl Pts',(0.631684198665438,-0.232861760990032,
0.750785745543687));
#14592=CARTESIAN_POINT('Ctrl Pts',(0.663382628119203,-0.244251601209411,
0.722929908501543));
#14593=CARTESIAN_POINT('Ctrl Pts',(0.679352081686668,-0.246942143572133,
0.707917883896095));
#14594=CARTESIAN_POINT('Ctrl Pts',(0.707917883896095,-0.246942143572133,
0.679352081686668));
#14595=CARTESIAN_POINT('Ctrl Pts',(0.722929908501543,-0.244251601209411,
0.663382628119203));
#14596=CARTESIAN_POINT('Ctrl Pts',(0.750785745543687,-0.232861760990032,
0.631684198665439));
#14597=CARTESIAN_POINT('Ctrl Pts',(0.763642258217232,-0.224161999508995,
0.615966552324775));
#14598=CARTESIAN_POINT('Ctrl Pts',(0.78555112003688,-0.203463743702801,
0.587792702767295));
#14599=CARTESIAN_POINT('Ctrl Pts',(0.795684265985088,-0.190326085855194,
0.573915184558108));
#14600=CARTESIAN_POINT('Ctrl Pts',(0.813159949759,-0.15976606450048,0.548874290046456));
#14601=CARTESIAN_POINT('Ctrl Pts',(0.820511285096538,-0.142345102874864,
0.537715343527944));
#14602=CARTESIAN_POINT('Ctrl Pts',(0.833661031856294,-0.099930567888331,
0.517157748491653));
#14603=CARTESIAN_POINT('Ctrl Pts',(0.838633903678357,-0.0740444353928835,
0.508899795931835));
#14604=CARTESIAN_POINT('Ctrl Pts',(0.841298510752801,-0.0476299999999999,
0.504455939115715));
#14605=CARTESIAN_POINT('',(0.528110872004958,-0.04763,0.871530771444223));
#14606=CARTESIAN_POINT('Origin',(0.707106781186547,-0.04763,0.707106781186548));
#14607=CARTESIAN_POINT('',(0.871530771444223,-0.04763,0.528110872004959));
#14608=CARTESIAN_POINT('Ctrl Pts',(0.871530771444223,-0.0476300000000001,
0.528110872004958));
#14609=CARTESIAN_POINT('Ctrl Pts',(0.87014664509073,-0.0609922781173483,
0.530395067942936));
#14610=CARTESIAN_POINT('Ctrl Pts',(0.868149331745851,-0.0742967091364493,
0.533674141594226));
#14611=CARTESIAN_POINT('Ctrl Pts',(0.85981294420286,-0.115492077056649,
0.54708917182331));
#14612=CARTESIAN_POINT('Ctrl Pts',(0.850993704737257,-0.141695629206859,
0.560922177770136));
#14613=CARTESIAN_POINT('Ctrl Pts',(0.830754510485543,-0.181890537957859,
0.590422647829571));
#14614=CARTESIAN_POINT('Ctrl Pts',(0.816896541396381,-0.201072148666545,
0.609616703125488));
#14615=CARTESIAN_POINT('Ctrl Pts',(0.792310597819928,-0.223955109275652,
0.641117951819998));
#14616=CARTESIAN_POINT('Ctrl Pts',(0.779109323683612,-0.232742381310829,
0.657208095763053));
#14617=CARTESIAN_POINT('Ctrl Pts',(0.750552691816206,-0.244234834628584,
0.68964083160521));
#14618=CARTESIAN_POINT('Ctrl Pts',(0.735185187071673,-0.246942143572133,
0.705971972091755));
#14619=CARTESIAN_POINT('Ctrl Pts',(0.705971972091754,-0.246942143572133,
0.735185187071673));
#14620=CARTESIAN_POINT('Ctrl Pts',(0.689640831605209,-0.244234834628584,
0.750552691816206));
#14621=CARTESIAN_POINT('Ctrl Pts',(0.657208095763052,-0.232742381310829,
0.779109323683612));
#14622=CARTESIAN_POINT('Ctrl Pts',(0.641117951819998,-0.223955109275652,
0.792310597819928));
#14623=CARTESIAN_POINT('Ctrl Pts',(0.609616703125487,-0.201072148666545,
0.816896541396382));
#14624=CARTESIAN_POINT('Ctrl Pts',(0.590422647829571,-0.181890537957858,
0.830754510485544));
#14625=CARTESIAN_POINT('Ctrl Pts',(0.560922177770135,-0.141695629206858,
0.850993704737257));
#14626=CARTESIAN_POINT('Ctrl Pts',(0.547089171823309,-0.115492077056649,
0.859812944202861));
#14627=CARTESIAN_POINT('Ctrl Pts',(0.533674141594226,-0.0742967091364491,
0.868149331745852));
#14628=CARTESIAN_POINT('Ctrl Pts',(0.530395067942936,-0.0609922781173483,
0.870146645090731));
#14629=CARTESIAN_POINT('Ctrl Pts',(0.528110872004958,-0.0476300000000001,
0.871530771444223));
#14630=CARTESIAN_POINT('Origin',(0.707106781186547,-0.04763,0.707106781186548));
#14631=CARTESIAN_POINT('Origin',(0.,-0.166705,0.));
#14632=CARTESIAN_POINT('',(0.242834539687906,-0.04763,0.989696097314));
#14633=CARTESIAN_POINT('Origin',(0.,-0.04763,0.));
#14634=CARTESIAN_POINT('',(-0.242834539687907,-0.04763,0.989696097314));
#14635=CARTESIAN_POINT('Ctrl Pts',(0.242834539687906,-0.04763,0.989696097314));
#14636=CARTESIAN_POINT('Ctrl Pts',(0.24024064412003,-0.0609922781173483,
0.990332542620729));
#14637=CARTESIAN_POINT('Ctrl Pts',(0.236509675094874,-0.0742967091364492,
0.991238884025248));
#14638=CARTESIAN_POINT('Ctrl Pts',(0.221129100087819,-0.115492077056649,
0.994830026707808));
#14639=CARTESIAN_POINT('Ctrl Pts',(0.205111543747588,-0.141695629206859,
0.998375294985966));
#14640=CARTESIAN_POINT('Ctrl Pts',(0.169940289819232,-0.181890537957859,
1.00492400591205));
#14641=CARTESIAN_POINT('Ctrl Pts',(0.1465689792446,-0.201072148666545,1.00869718865384));
#14642=CARTESIAN_POINT('Ctrl Pts',(0.106909345252087,-0.223955109275652,
1.01358704779679));
#14643=CARTESIAN_POINT('Ctrl Pts',(0.0861971848975941,-0.232742381310829,
1.0156297872271));
#14644=CARTESIAN_POINT('Ctrl Pts',(0.0430711894098822,-0.244234834628584,
1.01837060663223));
#14645=CARTESIAN_POINT('Ctrl Pts',(0.0206568624125605,-0.246942143572133,
1.019052));
#14646=CARTESIAN_POINT('Ctrl Pts',(-0.0206568624125608,-0.246942143572133,
1.019052));
#14647=CARTESIAN_POINT('Ctrl Pts',(-0.0430711894098825,-0.244234834628584,
1.01837060663223));
#14648=CARTESIAN_POINT('Ctrl Pts',(-0.0861971848975943,-0.232742381310829,
1.0156297872271));
#14649=CARTESIAN_POINT('Ctrl Pts',(-0.106909345252088,-0.223955109275652,
1.01358704779679));
#14650=CARTESIAN_POINT('Ctrl Pts',(-0.1465689792446,-0.201072148666545,
1.00869718865384));
#14651=CARTESIAN_POINT('Ctrl Pts',(-0.169940289819232,-0.181890537957859,
1.00492400591205));
#14652=CARTESIAN_POINT('Ctrl Pts',(-0.205111543747588,-0.141695629206859,
0.998375294985966));
#14653=CARTESIAN_POINT('Ctrl Pts',(-0.221129100087819,-0.115492077056649,
0.994830026707808));
#14654=CARTESIAN_POINT('Ctrl Pts',(-0.236509675094875,-0.0742967091364493,
0.991238884025248));
#14655=CARTESIAN_POINT('Ctrl Pts',(-0.24024064412003,-0.0609922781173483,
0.990332542620729));
#14656=CARTESIAN_POINT('Ctrl Pts',(-0.242834539687907,-0.04763,0.989696097314));
#14657=CARTESIAN_POINT('',(-0.528110872004959,-0.04763,0.871530771444223));
#14658=CARTESIAN_POINT('Origin',(0.,-0.04763,0.));
#14659=CARTESIAN_POINT('',(-0.871530771444223,-0.04763,0.528110872004958));
#14660=CARTESIAN_POINT('Ctrl Pts',(-0.528110872004958,-0.0476300000000001,
0.871530771444223));
#14661=CARTESIAN_POINT('Ctrl Pts',(-0.530395067942936,-0.0609922781173484,
0.87014664509073));
#14662=CARTESIAN_POINT('Ctrl Pts',(-0.533674141594226,-0.0742967091364493,
0.868149331745851));
#14663=CARTESIAN_POINT('Ctrl Pts',(-0.54708917182331,-0.115492077056649,
0.85981294420286));
#14664=CARTESIAN_POINT('Ctrl Pts',(-0.560922177770136,-0.141695629206859,
0.850993704737257));
#14665=CARTESIAN_POINT('Ctrl Pts',(-0.590422647829571,-0.181890537957859,
0.830754510485543));
#14666=CARTESIAN_POINT('Ctrl Pts',(-0.609616703125488,-0.201072148666545,
0.816896541396381));
#14667=CARTESIAN_POINT('Ctrl Pts',(-0.641117951819998,-0.223955109275652,
0.792310597819928));
#14668=CARTESIAN_POINT('Ctrl Pts',(-0.657208095763053,-0.232742381310829,
0.779109323683611));
#14669=CARTESIAN_POINT('Ctrl Pts',(-0.68964083160521,-0.244234834628584,
0.750552691816205));
#14670=CARTESIAN_POINT('Ctrl Pts',(-0.705971972091755,-0.246942143572133,
0.735185187071673));
#14671=CARTESIAN_POINT('Ctrl Pts',(-0.735185187071673,-0.246942143572133,
0.705971972091754));
#14672=CARTESIAN_POINT('Ctrl Pts',(-0.750552691816206,-0.244234834628584,
0.689640831605209));
#14673=CARTESIAN_POINT('Ctrl Pts',(-0.779109323683612,-0.232742381310829,
0.657208095763052));
#14674=CARTESIAN_POINT('Ctrl Pts',(-0.792310597819928,-0.223955109275652,
0.641117951819998));
#14675=CARTESIAN_POINT('Ctrl Pts',(-0.816896541396382,-0.201072148666545,
0.609616703125487));
#14676=CARTESIAN_POINT('Ctrl Pts',(-0.830754510485544,-0.181890537957858,
0.590422647829571));
#14677=CARTESIAN_POINT('Ctrl Pts',(-0.850993704737257,-0.141695629206858,
0.560922177770135));
#14678=CARTESIAN_POINT('Ctrl Pts',(-0.859812944202861,-0.115492077056649,
0.547089171823309));
#14679=CARTESIAN_POINT('Ctrl Pts',(-0.868149331745852,-0.0742967091364491,
0.533674141594226));
#14680=CARTESIAN_POINT('Ctrl Pts',(-0.870146645090731,-0.0609922781173483,
0.530395067942936));
#14681=CARTESIAN_POINT('Ctrl Pts',(-0.871530771444223,-0.04763,0.528110872004958));
#14682=CARTESIAN_POINT('',(-0.989696097314,-0.04763,0.242834539687906));
#14683=CARTESIAN_POINT('Origin',(0.,-0.04763,0.));
#14684=CARTESIAN_POINT('',(-1.019052,-0.246942143572133,1.248489836334E-16));
#14685=CARTESIAN_POINT('Ctrl Pts',(-0.989696097314,-0.04763,0.242834539687906));
#14686=CARTESIAN_POINT('Ctrl Pts',(-0.990332542620729,-0.0609922781173483,
0.24024064412003));
#14687=CARTESIAN_POINT('Ctrl Pts',(-0.991238884025248,-0.0742967091364492,
0.236509675094874));
#14688=CARTESIAN_POINT('Ctrl Pts',(-0.994830026707808,-0.115492077056649,
0.221129100087819));
#14689=CARTESIAN_POINT('Ctrl Pts',(-0.998375294985966,-0.141695629206859,
0.205111543747588));
#14690=CARTESIAN_POINT('Ctrl Pts',(-1.00492400591205,-0.181890537957859,
0.169940289819232));
#14691=CARTESIAN_POINT('Ctrl Pts',(-1.00869718865384,-0.201072148666545,
0.1465689792446));
#14692=CARTESIAN_POINT('Ctrl Pts',(-1.01358704779679,-0.223955109275652,
0.106909345252088));
#14693=CARTESIAN_POINT('Ctrl Pts',(-1.0156297872271,-0.232742381310829,
0.0861971848975944));
#14694=CARTESIAN_POINT('Ctrl Pts',(-1.01837060663223,-0.244234834628584,
0.0430711894098825));
#14695=CARTESIAN_POINT('Ctrl Pts',(-1.019052,-0.246942143572133,0.0206568624125608));
#14696=CARTESIAN_POINT('Ctrl Pts',(-1.019052,-0.246942143572133,1.2490009027033E-16));
#14697=CARTESIAN_POINT('',(-1.019052,-0.28578,1.24797876996471E-16));
#14698=CARTESIAN_POINT('',(-1.019052,-0.166705,1.24797876996471E-16));
#14699=CARTESIAN_POINT('Origin',(0.,-0.28578,0.));
#14700=CARTESIAN_POINT('',(-0.989696097314,-0.04763,-0.242834539687906));
#14701=CARTESIAN_POINT('Ctrl Pts',(-1.019052,-0.246942143572133,1.2490009027033E-16));
#14702=CARTESIAN_POINT('Ctrl Pts',(-1.019052,-0.246942143572133,-0.0206568624125605));
#14703=CARTESIAN_POINT('Ctrl Pts',(-1.01837060663223,-0.244234834628584,
-0.0430711894098822));
#14704=CARTESIAN_POINT('Ctrl Pts',(-1.0156297872271,-0.232742381310829,
-0.0861971848975941));
#14705=CARTESIAN_POINT('Ctrl Pts',(-1.01358704779679,-0.223955109275652,
-0.106909345252087));
#14706=CARTESIAN_POINT('Ctrl Pts',(-1.00869718865384,-0.201072148666546,
-0.1465689792446));
#14707=CARTESIAN_POINT('Ctrl Pts',(-1.00492400591205,-0.181890537957859,
-0.169940289819232));
#14708=CARTESIAN_POINT('Ctrl Pts',(-0.998375294985966,-0.141695629206859,
-0.205111543747588));
#14709=CARTESIAN_POINT('Ctrl Pts',(-0.994830026707808,-0.11549207705665,
-0.221129100087819));
#14710=CARTESIAN_POINT('Ctrl Pts',(-0.991238884025248,-0.0742967091364495,
-0.236509675094874));
#14711=CARTESIAN_POINT('Ctrl Pts',(-0.990332542620729,-0.0609922781173484,
-0.24024064412003));
#14712=CARTESIAN_POINT('Ctrl Pts',(-0.989696097314,-0.0476300000000001,
-0.242834539687907));
#14713=CARTESIAN_POINT('',(-0.871530771444223,-0.04763,-0.528110872004958));
#14714=CARTESIAN_POINT('Origin',(0.,-0.04763,0.));
#14715=CARTESIAN_POINT('',(-0.528110872004958,-0.04763,-0.871530771444223));
#14716=CARTESIAN_POINT('Ctrl Pts',(-0.871530771444223,-0.0476300000000001,
-0.528110872004958));
#14717=CARTESIAN_POINT('Ctrl Pts',(-0.87014664509073,-0.0609922781173484,
-0.530395067942936));
#14718=CARTESIAN_POINT('Ctrl Pts',(-0.868149331745851,-0.0742967091364494,
-0.533674141594226));
#14719=CARTESIAN_POINT('Ctrl Pts',(-0.85981294420286,-0.115492077056649,
-0.54708917182331));
#14720=CARTESIAN_POINT('Ctrl Pts',(-0.850993704737257,-0.141695629206859,
-0.560922177770136));
#14721=CARTESIAN_POINT('Ctrl Pts',(-0.830754510485543,-0.181890537957859,
-0.590422647829571));
#14722=CARTESIAN_POINT('Ctrl Pts',(-0.816896541396381,-0.201072148666546,
-0.609616703125488));
#14723=CARTESIAN_POINT('Ctrl Pts',(-0.792310597819928,-0.223955109275652,
-0.641117951819999));
#14724=CARTESIAN_POINT('Ctrl Pts',(-0.779109323683611,-0.232742381310829,
-0.657208095763053));
#14725=CARTESIAN_POINT('Ctrl Pts',(-0.750552691816205,-0.244234834628584,
-0.68964083160521));
#14726=CARTESIAN_POINT('Ctrl Pts',(-0.735185187071673,-0.246942143572133,
-0.705971972091755));
#14727=CARTESIAN_POINT('Ctrl Pts',(-0.705971972091754,-0.246942143572133,
-0.735185187071673));
#14728=CARTESIAN_POINT('Ctrl Pts',(-0.68964083160521,-0.244234834628584,
-0.750552691816206));
#14729=CARTESIAN_POINT('Ctrl Pts',(-0.657208095763052,-0.232742381310829,
-0.779109323683612));
#14730=CARTESIAN_POINT('Ctrl Pts',(-0.641117951819998,-0.223955109275652,
-0.792310597819928));
#14731=CARTESIAN_POINT('Ctrl Pts',(-0.609616703125488,-0.201072148666545,
-0.816896541396381));
#14732=CARTESIAN_POINT('Ctrl Pts',(-0.590422647829571,-0.181890537957859,
-0.830754510485543));
#14733=CARTESIAN_POINT('Ctrl Pts',(-0.560922177770136,-0.141695629206859,
-0.850993704737257));
#14734=CARTESIAN_POINT('Ctrl Pts',(-0.54708917182331,-0.115492077056649,
-0.85981294420286));
#14735=CARTESIAN_POINT('Ctrl Pts',(-0.533674141594226,-0.0742967091364494,
-0.868149331745852));
#14736=CARTESIAN_POINT('Ctrl Pts',(-0.530395067942936,-0.0609922781173484,
-0.870146645090731));
#14737=CARTESIAN_POINT('Ctrl Pts',(-0.528110872004958,-0.0476300000000001,
-0.871530771444223));
#14738=CARTESIAN_POINT('',(-0.242834539687906,-0.04763,-0.989696097314));
#14739=CARTESIAN_POINT('Origin',(0.,-0.04763,0.));
#14740=CARTESIAN_POINT('',(0.242834539687906,-0.04763,-0.989696097314));
#14741=CARTESIAN_POINT('Ctrl Pts',(-0.242834539687907,-0.04763,-0.989696097314));
#14742=CARTESIAN_POINT('Ctrl Pts',(-0.24024064412003,-0.0609922781173483,
-0.990332542620729));
#14743=CARTESIAN_POINT('Ctrl Pts',(-0.236509675094874,-0.0742967091364493,
-0.991238884025248));
#14744=CARTESIAN_POINT('Ctrl Pts',(-0.221129100087819,-0.115492077056649,
-0.994830026707808));
#14745=CARTESIAN_POINT('Ctrl Pts',(-0.205111543747588,-0.141695629206859,
-0.998375294985966));
#14746=CARTESIAN_POINT('Ctrl Pts',(-0.169940289819232,-0.181890537957859,
-1.00492400591205));
#14747=CARTESIAN_POINT('Ctrl Pts',(-0.1465689792446,-0.201072148666545,
-1.00869718865384));
#14748=CARTESIAN_POINT('Ctrl Pts',(-0.106909345252087,-0.223955109275652,
-1.01358704779679));
#14749=CARTESIAN_POINT('Ctrl Pts',(-0.0861971848975942,-0.232742381310829,
-1.0156297872271));
#14750=CARTESIAN_POINT('Ctrl Pts',(-0.0430711894098823,-0.244234834628584,
-1.01837060663223));
#14751=CARTESIAN_POINT('Ctrl Pts',(-0.0206568624125606,-0.246942143572133,
-1.019052));
#14752=CARTESIAN_POINT('Ctrl Pts',(0.0206568624125607,-0.246942143572133,
-1.019052));
#14753=CARTESIAN_POINT('Ctrl Pts',(0.0430711894098824,-0.244234834628584,
-1.01837060663223));
#14754=CARTESIAN_POINT('Ctrl Pts',(0.0861971848975943,-0.232742381310829,
-1.0156297872271));
#14755=CARTESIAN_POINT('Ctrl Pts',(0.106909345252088,-0.223955109275652,
-1.01358704779679));
#14756=CARTESIAN_POINT('Ctrl Pts',(0.1465689792446,-0.201072148666545,-1.00869718865384));
#14757=CARTESIAN_POINT('Ctrl Pts',(0.169940289819232,-0.181890537957859,
-1.00492400591205));
#14758=CARTESIAN_POINT('Ctrl Pts',(0.205111543747588,-0.141695629206859,
-0.998375294985966));
#14759=CARTESIAN_POINT('Ctrl Pts',(0.221129100087819,-0.115492077056649,
-0.994830026707808));
#14760=CARTESIAN_POINT('Ctrl Pts',(0.236509675094874,-0.0742967091364493,
-0.991238884025248));
#14761=CARTESIAN_POINT('Ctrl Pts',(0.24024064412003,-0.0609922781173484,
-0.990332542620729));
#14762=CARTESIAN_POINT('Ctrl Pts',(0.242834539687907,-0.04763,-0.989696097314));
#14763=CARTESIAN_POINT('',(0.528110872004958,-0.04763,-0.871530771444223));
#14764=CARTESIAN_POINT('Origin',(0.,-0.04763,0.));
#14765=CARTESIAN_POINT('',(0.871530771444223,-0.04763,-0.528110872004958));
#14766=CARTESIAN_POINT('Ctrl Pts',(0.528110872004958,-0.0476300000000001,
-0.871530771444223));
#14767=CARTESIAN_POINT('Ctrl Pts',(0.530395067942936,-0.0609922781173484,
-0.870146645090731));
#14768=CARTESIAN_POINT('Ctrl Pts',(0.533674141594226,-0.0742967091364493,
-0.868149331745851));
#14769=CARTESIAN_POINT('Ctrl Pts',(0.54708917182331,-0.115492077056649,
-0.85981294420286));
#14770=CARTESIAN_POINT('Ctrl Pts',(0.560922177770136,-0.141695629206859,
-0.850993704737257));
#14771=CARTESIAN_POINT('Ctrl Pts',(0.590422647829571,-0.181890537957859,
-0.830754510485543));
#14772=CARTESIAN_POINT('Ctrl Pts',(0.609616703125488,-0.201072148666545,
-0.816896541396381));
#14773=CARTESIAN_POINT('Ctrl Pts',(0.641117951819998,-0.223955109275652,
-0.792310597819928));
#14774=CARTESIAN_POINT('Ctrl Pts',(0.657208095763053,-0.232742381310829,
-0.779109323683612));
#14775=CARTESIAN_POINT('Ctrl Pts',(0.68964083160521,-0.244234834628584,
-0.750552691816206));
#14776=CARTESIAN_POINT('Ctrl Pts',(0.705971972091755,-0.246942143572133,
-0.735185187071673));
#14777=CARTESIAN_POINT('Ctrl Pts',(0.735185187071673,-0.246942143572133,
-0.705971972091754));
#14778=CARTESIAN_POINT('Ctrl Pts',(0.750552691816206,-0.244234834628584,
-0.68964083160521));
#14779=CARTESIAN_POINT('Ctrl Pts',(0.779109323683612,-0.232742381310829,
-0.657208095763053));
#14780=CARTESIAN_POINT('Ctrl Pts',(0.792310597819928,-0.223955109275652,
-0.641117951819998));
#14781=CARTESIAN_POINT('Ctrl Pts',(0.816896541396381,-0.201072148666545,
-0.609616703125488));
#14782=CARTESIAN_POINT('Ctrl Pts',(0.830754510485543,-0.181890537957859,
-0.590422647829571));
#14783=CARTESIAN_POINT('Ctrl Pts',(0.850993704737257,-0.141695629206859,
-0.560922177770136));
#14784=CARTESIAN_POINT('Ctrl Pts',(0.85981294420286,-0.115492077056649,
-0.54708917182331));
#14785=CARTESIAN_POINT('Ctrl Pts',(0.868149331745851,-0.0742967091364493,
-0.533674141594226));
#14786=CARTESIAN_POINT('Ctrl Pts',(0.870146645090731,-0.0609922781173484,
-0.530395067942936));
#14787=CARTESIAN_POINT('Ctrl Pts',(0.871530771444223,-0.0476300000000001,
-0.528110872004958));
#14788=CARTESIAN_POINT('',(0.989696097314,-0.04763,-0.242834539687906));
#14789=CARTESIAN_POINT('Origin',(0.,-0.04763,0.));
#14790=CARTESIAN_POINT('',(0.989696097314,-0.04763,0.242834539687906));
#14791=CARTESIAN_POINT('Ctrl Pts',(0.989696097314,-0.04763,-0.242834539687907));
#14792=CARTESIAN_POINT('Ctrl Pts',(0.990332542620729,-0.0609922781173483,
-0.24024064412003));
#14793=CARTESIAN_POINT('Ctrl Pts',(0.991238884025248,-0.0742967091364493,
-0.236509675094874));
#14794=CARTESIAN_POINT('Ctrl Pts',(0.994830026707808,-0.115492077056649,
-0.221129100087819));
#14795=CARTESIAN_POINT('Ctrl Pts',(0.998375294985966,-0.141695629206859,
-0.205111543747588));
#14796=CARTESIAN_POINT('Ctrl Pts',(1.00492400591205,-0.181890537957859,
-0.169940289819232));
#14797=CARTESIAN_POINT('Ctrl Pts',(1.00869718865384,-0.201072148666545,
-0.1465689792446));
#14798=CARTESIAN_POINT('Ctrl Pts',(1.01358704779679,-0.223955109275652,
-0.106909345252087));
#14799=CARTESIAN_POINT('Ctrl Pts',(1.0156297872271,-0.232742381310829,-0.0861971848975942));
#14800=CARTESIAN_POINT('Ctrl Pts',(1.01837060663223,-0.244234834628584,
-0.0430711894098823));
#14801=CARTESIAN_POINT('Ctrl Pts',(1.019052,-0.246942143572133,-0.0206568624125607));
#14802=CARTESIAN_POINT('Ctrl Pts',(1.019052,-0.246942143572133,0.0206568624125607));
#14803=CARTESIAN_POINT('Ctrl Pts',(1.01837060663223,-0.244234834628584,
0.0430711894098823));
#14804=CARTESIAN_POINT('Ctrl Pts',(1.0156297872271,-0.232742381310829,0.0861971848975942));
#14805=CARTESIAN_POINT('Ctrl Pts',(1.01358704779679,-0.223955109275652,
0.106909345252087));
#14806=CARTESIAN_POINT('Ctrl Pts',(1.00869718865384,-0.201072148666545,
0.1465689792446));
#14807=CARTESIAN_POINT('Ctrl Pts',(1.00492400591205,-0.181890537957859,
0.169940289819232));
#14808=CARTESIAN_POINT('Ctrl Pts',(0.998375294985966,-0.141695629206859,
0.205111543747588));
#14809=CARTESIAN_POINT('Ctrl Pts',(0.994830026707808,-0.115492077056649,
0.221129100087819));
#14810=CARTESIAN_POINT('Ctrl Pts',(0.991238884025248,-0.0742967091364492,
0.236509675094874));
#14811=CARTESIAN_POINT('Ctrl Pts',(0.990332542620729,-0.0609922781173483,
0.24024064412003));
#14812=CARTESIAN_POINT('Ctrl Pts',(0.989696097314,-0.04763,0.242834539687907));
#14813=CARTESIAN_POINT('Origin',(0.,-0.04763,0.));
#14814=CARTESIAN_POINT('Origin',(0.,-0.04763,0.));
#14815=CARTESIAN_POINT('',(0.238183666596899,-0.04763,0.951592097314));
#14816=CARTESIAN_POINT('Origin',(0.,-0.04763,0.));
#14817=CARTESIAN_POINT('Origin',(-1.94289029309402E-16,-0.04763,1.));
#14818=CARTESIAN_POINT('Origin',(-1.94289029309402E-16,0.,1.));
#14819=CARTESIAN_POINT('',(-0.2381836665969,-0.04763,0.951592097314));
#14820=CARTESIAN_POINT('Ctrl Pts',(-0.238183666596899,-0.0476299999999999,
0.951592097314));
#14821=CARTESIAN_POINT('Ctrl Pts',(-0.233157223576062,-0.0740444353928835,
0.952850216871763));
#14822=CARTESIAN_POINT('Ctrl Pts',(-0.223801617934946,-0.0999305678883309,
0.955173119738174));
#14823=CARTESIAN_POINT('Ctrl Pts',(-0.199966927975188,-0.142345102874864,
0.960411259488514));
#14824=CARTESIAN_POINT('Ctrl Pts',(-0.1868781821531,-0.159766064500479,
0.963103647174702));
#14825=CARTESIAN_POINT('Ctrl Pts',(-0.15681442133453,-0.190326085855194,
0.968453058988463));
#14826=CARTESIAN_POINT('Ctrl Pts',(-0.139836317888043,-0.203463743702801,
0.971100730005489));
#14827=CARTESIAN_POINT('Ctrl Pts',(-0.104422493053067,-0.224161999508995,
0.975530745318961));
#14828=CARTESIAN_POINT('Ctrl Pts',(-0.0842175114474176,-0.232861760990032,
0.977553872336861));
#14829=CARTESIAN_POINT('Ctrl Pts',(-0.0421062857595701,-0.244251601209411,
0.980270995488453));
#14830=CARTESIAN_POINT('Ctrl Pts',(-0.0201990724523197,-0.246942143572133,
0.980948));
#14831=CARTESIAN_POINT('Ctrl Pts',(0.020199072452319,-0.246942143572133,
0.980948));
#14832=CARTESIAN_POINT('Ctrl Pts',(0.0421062857595694,-0.244251601209411,
0.980270995488454));
#14833=CARTESIAN_POINT('Ctrl Pts',(0.0842175114474169,-0.232861760990032,
0.977553872336861));
#14834=CARTESIAN_POINT('Ctrl Pts',(0.104422493053067,-0.224161999508995,
0.975530745318961));
#14835=CARTESIAN_POINT('Ctrl Pts',(0.139836317888042,-0.203463743702801,
0.971100730005489));
#14836=CARTESIAN_POINT('Ctrl Pts',(0.15681442133453,-0.190326085855194,
0.968453058988463));
#14837=CARTESIAN_POINT('Ctrl Pts',(0.1868781821531,-0.15976606450048,0.963103647174702));
#14838=CARTESIAN_POINT('Ctrl Pts',(0.199966927975188,-0.142345102874864,
0.960411259488514));
#14839=CARTESIAN_POINT('Ctrl Pts',(0.223801617934945,-0.0999305678883309,
0.955173119738174));
#14840=CARTESIAN_POINT('Ctrl Pts',(0.233157223576061,-0.0740444353928835,
0.952850216871763));
#14841=CARTESIAN_POINT('Ctrl Pts',(0.238183666596899,-0.0476299999999999,
0.951592097314));
#14842=CARTESIAN_POINT('Origin',(-1.94289029309402E-16,-0.04763,1.));
#14843=CARTESIAN_POINT('Origin',(0.,-0.04763,0.));
#14844=CARTESIAN_POINT('',(-0.504455939115715,-0.04763,0.841298510752802));
#14845=CARTESIAN_POINT('Origin',(0.,-0.04763,0.));
#14846=CARTESIAN_POINT('Origin',(-0.707106781186548,-0.04763,0.707106781186547));
#14847=CARTESIAN_POINT('Origin',(-0.707106781186548,0.,0.707106781186547));
#14848=CARTESIAN_POINT('',(-0.841298510752802,-0.04763,0.504455939115715));
#14849=CARTESIAN_POINT('Ctrl Pts',(-0.841298510752802,-0.04763,0.504455939115715));
#14850=CARTESIAN_POINT('Ctrl Pts',(-0.838633903678357,-0.0740444353928835,
0.508899795931835));
#14851=CARTESIAN_POINT('Ctrl Pts',(-0.833661031856294,-0.0999305678883309,
0.517157748491652));
#14852=CARTESIAN_POINT('Ctrl Pts',(-0.820511285096538,-0.142345102874864,
0.537715343527944));
#14853=CARTESIAN_POINT('Ctrl Pts',(-0.813159949759,-0.159766064500479,0.548874290046456));
#14854=CARTESIAN_POINT('Ctrl Pts',(-0.795684265985089,-0.190326085855194,
0.573915184558107));
#14855=CARTESIAN_POINT('Ctrl Pts',(-0.78555112003688,-0.203463743702801,
0.587792702767295));
#14856=CARTESIAN_POINT('Ctrl Pts',(-0.763642258217233,-0.224161999508995,
0.615966552324775));
#14857=CARTESIAN_POINT('Ctrl Pts',(-0.750785745543687,-0.232861760990032,
0.631684198665438));
#14858=CARTESIAN_POINT('Ctrl Pts',(-0.722929908501543,-0.244251601209411,
0.663382628119203));
#14859=CARTESIAN_POINT('Ctrl Pts',(-0.707917883896095,-0.246942143572133,
0.679352081686668));
#14860=CARTESIAN_POINT('Ctrl Pts',(-0.679352081686668,-0.246942143572133,
0.707917883896095));
#14861=CARTESIAN_POINT('Ctrl Pts',(-0.663382628119203,-0.244251601209411,
0.722929908501544));
#14862=CARTESIAN_POINT('Ctrl Pts',(-0.631684198665438,-0.232861760990031,
0.750785745543687));
#14863=CARTESIAN_POINT('Ctrl Pts',(-0.615966552324775,-0.224161999508995,
0.763642258217233));
#14864=CARTESIAN_POINT('Ctrl Pts',(-0.587792702767295,-0.203463743702801,
0.78555112003688));
#14865=CARTESIAN_POINT('Ctrl Pts',(-0.573915184558107,-0.190326085855194,
0.795684265985088));
#14866=CARTESIAN_POINT('Ctrl Pts',(-0.548874290046456,-0.159766064500479,
0.813159949759));
#14867=CARTESIAN_POINT('Ctrl Pts',(-0.537715343527944,-0.142345102874864,
0.820511285096538));
#14868=CARTESIAN_POINT('Ctrl Pts',(-0.517157748491652,-0.0999305678883309,
0.833661031856294));
#14869=CARTESIAN_POINT('Ctrl Pts',(-0.508899795931835,-0.0740444353928835,
0.838633903678357));
#14870=CARTESIAN_POINT('Ctrl Pts',(-0.504455939115716,-0.04763,0.841298510752801));
#14871=CARTESIAN_POINT('Origin',(-0.707106781186548,-0.04763,0.707106781186547));
#14872=CARTESIAN_POINT('Origin',(0.,-0.04763,0.));
#14873=CARTESIAN_POINT('',(-0.951592097314,-0.04763,0.238183666596899));
#14874=CARTESIAN_POINT('Origin',(0.,-0.04763,0.));
#14875=CARTESIAN_POINT('Origin',(-1.,-0.04763,-1.11022302462516E-16));
#14876=CARTESIAN_POINT('Origin',(-1.,0.,-1.11022302462516E-16));
#14877=CARTESIAN_POINT('',(-0.951592097314,-0.04763,-0.2381836665969));
#14878=CARTESIAN_POINT('',(-0.980948,-0.246942143572133,1.08514323328844E-18));
#14879=CARTESIAN_POINT('Ctrl Pts',(-0.951592097314,-0.04763,-0.238183666596899));
#14880=CARTESIAN_POINT('Ctrl Pts',(-0.952850216871763,-0.0740444353928835,
-0.233157223576062));
#14881=CARTESIAN_POINT('Ctrl Pts',(-0.955173119738174,-0.0999305678883309,
-0.223801617934946));
#14882=CARTESIAN_POINT('Ctrl Pts',(-0.960411259488514,-0.142345102874864,
-0.199966927975188));
#14883=CARTESIAN_POINT('Ctrl Pts',(-0.963103647174702,-0.159766064500479,
-0.1868781821531));
#14884=CARTESIAN_POINT('Ctrl Pts',(-0.968453058988463,-0.190326085855194,
-0.15681442133453));
#14885=CARTESIAN_POINT('Ctrl Pts',(-0.971100730005489,-0.203463743702801,
-0.139836317888043));
#14886=CARTESIAN_POINT('Ctrl Pts',(-0.975530745318961,-0.224161999508995,
-0.104422493053067));
#14887=CARTESIAN_POINT('Ctrl Pts',(-0.977553872336861,-0.232861760990032,
-0.0842175114474175));
#14888=CARTESIAN_POINT('Ctrl Pts',(-0.980270995488453,-0.244251601209411,
-0.0421062857595699));
#14889=CARTESIAN_POINT('Ctrl Pts',(-0.980948,-0.246942143572133,-0.0201990724523195));
#14890=CARTESIAN_POINT('Ctrl Pts',(-0.980948,-0.246942143572133,-1.17961196366423E-16));
#14891=CARTESIAN_POINT('Origin',(-1.,-0.04763,-1.11022302462516E-16));
#14892=CARTESIAN_POINT('Ctrl Pts',(-0.980948,-0.246942143572133,-1.17961196366423E-16));
#14893=CARTESIAN_POINT('Ctrl Pts',(-0.980948,-0.246942143572133,0.0201990724523192));
#14894=CARTESIAN_POINT('Ctrl Pts',(-0.980270995488453,-0.244251601209411,
0.0421062857595695));
#14895=CARTESIAN_POINT('Ctrl Pts',(-0.977553872336861,-0.232861760990032,
0.0842175114474169));
#14896=CARTESIAN_POINT('Ctrl Pts',(-0.975530745318961,-0.224161999508995,
0.104422493053066));
#14897=CARTESIAN_POINT('Ctrl Pts',(-0.971100730005489,-0.203463743702801,
0.139836317888042));
#14898=CARTESIAN_POINT('Ctrl Pts',(-0.968453058988463,-0.190326085855194,
0.15681442133453));
#14899=CARTESIAN_POINT('Ctrl Pts',(-0.963103647174702,-0.15976606450048,
0.1868781821531));
#14900=CARTESIAN_POINT('Ctrl Pts',(-0.960411259488514,-0.142345102874864,
0.199966927975188));
#14901=CARTESIAN_POINT('Ctrl Pts',(-0.955173119738174,-0.099930567888331,
0.223801617934945));
#14902=CARTESIAN_POINT('Ctrl Pts',(-0.952850216871763,-0.0740444353928835,
0.233157223576061));
#14903=CARTESIAN_POINT('Ctrl Pts',(-0.951592097314,-0.04763,0.238183666596899));
#14904=CARTESIAN_POINT('Origin',(0.,-0.04763,0.));
#14905=CARTESIAN_POINT('',(-0.841298510752802,-0.04763,-0.504455939115715));
#14906=CARTESIAN_POINT('Origin',(0.,-0.04763,0.));
#14907=CARTESIAN_POINT('Origin',(-0.707106781186547,-0.04763,-0.707106781186548));
#14908=CARTESIAN_POINT('Origin',(-0.707106781186547,0.,-0.707106781186548));
#14909=CARTESIAN_POINT('',(-0.504455939115715,-0.04763,-0.841298510752802));
#14910=CARTESIAN_POINT('Ctrl Pts',(-0.504455939115715,-0.04763,-0.841298510752802));
#14911=CARTESIAN_POINT('Ctrl Pts',(-0.508899795931835,-0.0740444353928835,
-0.838633903678357));
#14912=CARTESIAN_POINT('Ctrl Pts',(-0.517157748491652,-0.0999305678883309,
-0.833661031856294));
#14913=CARTESIAN_POINT('Ctrl Pts',(-0.537715343527944,-0.142345102874864,
-0.820511285096538));
#14914=CARTESIAN_POINT('Ctrl Pts',(-0.548874290046456,-0.159766064500479,
-0.813159949759));
#14915=CARTESIAN_POINT('Ctrl Pts',(-0.573915184558107,-0.190326085855194,
-0.795684265985089));
#14916=CARTESIAN_POINT('Ctrl Pts',(-0.587792702767295,-0.203463743702801,
-0.78555112003688));
#14917=CARTESIAN_POINT('Ctrl Pts',(-0.615966552324775,-0.224161999508995,
-0.763642258217233));
#14918=CARTESIAN_POINT('Ctrl Pts',(-0.631684198665438,-0.232861760990032,
-0.750785745543687));
#14919=CARTESIAN_POINT('Ctrl Pts',(-0.663382628119203,-0.244251601209411,
-0.722929908501543));
#14920=CARTESIAN_POINT('Ctrl Pts',(-0.679352081686668,-0.246942143572133,
-0.707917883896095));
#14921=CARTESIAN_POINT('Ctrl Pts',(-0.707917883896095,-0.246942143572133,
-0.679352081686668));
#14922=CARTESIAN_POINT('Ctrl Pts',(-0.722929908501543,-0.244251601209411,
-0.663382628119203));
#14923=CARTESIAN_POINT('Ctrl Pts',(-0.750785745543687,-0.232861760990032,
-0.631684198665439));
#14924=CARTESIAN_POINT('Ctrl Pts',(-0.763642258217232,-0.224161999508995,
-0.615966552324775));
#14925=CARTESIAN_POINT('Ctrl Pts',(-0.78555112003688,-0.203463743702801,
-0.587792702767295));
#14926=CARTESIAN_POINT('Ctrl Pts',(-0.795684265985088,-0.190326085855194,
-0.573915184558107));
#14927=CARTESIAN_POINT('Ctrl Pts',(-0.813159949759,-0.15976606450048,-0.548874290046456));
#14928=CARTESIAN_POINT('Ctrl Pts',(-0.820511285096538,-0.142345102874864,
-0.537715343527944));
#14929=CARTESIAN_POINT('Ctrl Pts',(-0.833661031856294,-0.0999305678883311,
-0.517157748491652));
#14930=CARTESIAN_POINT('Ctrl Pts',(-0.838633903678357,-0.0740444353928836,
-0.508899795931835));
#14931=CARTESIAN_POINT('Ctrl Pts',(-0.841298510752801,-0.04763,-0.504455939115715));
#14932=CARTESIAN_POINT('Origin',(-0.707106781186547,-0.04763,-0.707106781186548));
#14933=CARTESIAN_POINT('Origin',(0.,-0.04763,0.));
#14934=CARTESIAN_POINT('',(-0.238183666596899,-0.04763,-0.951592097314));
#14935=CARTESIAN_POINT('Origin',(0.,-0.04763,0.));
#14936=CARTESIAN_POINT('Origin',(5.55111512312578E-17,-0.04763,-1.));
#14937=CARTESIAN_POINT('Origin',(5.55111512312578E-17,0.,-1.));
#14938=CARTESIAN_POINT('',(0.238183666596899,-0.04763,-0.951592097314));
#14939=CARTESIAN_POINT('Ctrl Pts',(0.238183666596899,-0.04763,-0.951592097314));
#14940=CARTESIAN_POINT('Ctrl Pts',(0.233157223576062,-0.0740444353928835,
-0.952850216871763));
#14941=CARTESIAN_POINT('Ctrl Pts',(0.223801617934946,-0.099930567888331,
-0.955173119738174));
#14942=CARTESIAN_POINT('Ctrl Pts',(0.199966927975188,-0.142345102874864,
-0.960411259488514));
#14943=CARTESIAN_POINT('Ctrl Pts',(0.1868781821531,-0.15976606450048,-0.963103647174702));
#14944=CARTESIAN_POINT('Ctrl Pts',(0.15681442133453,-0.190326085855194,
-0.968453058988463));
#14945=CARTESIAN_POINT('Ctrl Pts',(0.139836317888042,-0.203463743702801,
-0.971100730005489));
#14946=CARTESIAN_POINT('Ctrl Pts',(0.104422493053067,-0.224161999508995,
-0.975530745318961));
#14947=CARTESIAN_POINT('Ctrl Pts',(0.0842175114474173,-0.232861760990032,
-0.977553872336861));
#14948=CARTESIAN_POINT('Ctrl Pts',(0.0421062857595698,-0.244251601209411,
-0.980270995488453));
#14949=CARTESIAN_POINT('Ctrl Pts',(0.0201990724523194,-0.246942143572133,
-0.980948));
#14950=CARTESIAN_POINT('Ctrl Pts',(-0.0201990724523193,-0.246942143572133,
-0.980948));
#14951=CARTESIAN_POINT('Ctrl Pts',(-0.0421062857595697,-0.244251601209411,
-0.980270995488453));
#14952=CARTESIAN_POINT('Ctrl Pts',(-0.0842175114474171,-0.232861760990032,
-0.977553872336861));
#14953=CARTESIAN_POINT('Ctrl Pts',(-0.104422493053067,-0.224161999508995,
-0.975530745318961));
#14954=CARTESIAN_POINT('Ctrl Pts',(-0.139836317888042,-0.203463743702801,
-0.971100730005489));
#14955=CARTESIAN_POINT('Ctrl Pts',(-0.15681442133453,-0.190326085855194,
-0.968453058988463));
#14956=CARTESIAN_POINT('Ctrl Pts',(-0.1868781821531,-0.15976606450048,-0.963103647174702));
#14957=CARTESIAN_POINT('Ctrl Pts',(-0.199966927975188,-0.142345102874864,
-0.960411259488514));
#14958=CARTESIAN_POINT('Ctrl Pts',(-0.223801617934945,-0.099930567888331,
-0.955173119738174));
#14959=CARTESIAN_POINT('Ctrl Pts',(-0.233157223576062,-0.0740444353928835,
-0.952850216871763));
#14960=CARTESIAN_POINT('Ctrl Pts',(-0.238183666596899,-0.0476299999999999,
-0.951592097314));
#14961=CARTESIAN_POINT('Origin',(5.55111512312578E-17,-0.04763,-1.));
#14962=CARTESIAN_POINT('Origin',(0.,-0.04763,0.));
#14963=CARTESIAN_POINT('',(0.504455939115715,-0.04763,-0.841298510752802));
#14964=CARTESIAN_POINT('Origin',(0.,-0.04763,0.));
#14965=CARTESIAN_POINT('Origin',(0.707106781186548,-0.04763,-0.707106781186547));
#14966=CARTESIAN_POINT('Origin',(0.707106781186548,0.,-0.707106781186547));
#14967=CARTESIAN_POINT('',(0.841298510752802,-0.04763,-0.504455939115715));
#14968=CARTESIAN_POINT('Ctrl Pts',(0.841298510752802,-0.04763,-0.504455939115715));
#14969=CARTESIAN_POINT('Ctrl Pts',(0.838633903678357,-0.0740444353928835,
-0.508899795931835));
#14970=CARTESIAN_POINT('Ctrl Pts',(0.833661031856294,-0.0999305678883309,
-0.517157748491652));
#14971=CARTESIAN_POINT('Ctrl Pts',(0.820511285096538,-0.142345102874864,
-0.537715343527944));
#14972=CARTESIAN_POINT('Ctrl Pts',(0.813159949759,-0.159766064500479,-0.548874290046456));
#14973=CARTESIAN_POINT('Ctrl Pts',(0.795684265985088,-0.190326085855194,
-0.573915184558107));
#14974=CARTESIAN_POINT('Ctrl Pts',(0.78555112003688,-0.203463743702801,
-0.587792702767295));
#14975=CARTESIAN_POINT('Ctrl Pts',(0.763642258217233,-0.224161999508995,
-0.615966552324775));
#14976=CARTESIAN_POINT('Ctrl Pts',(0.750785745543687,-0.232861760990032,
-0.631684198665438));
#14977=CARTESIAN_POINT('Ctrl Pts',(0.722929908501543,-0.244251601209411,
-0.663382628119203));
#14978=CARTESIAN_POINT('Ctrl Pts',(0.707917883896095,-0.246942143572133,
-0.679352081686668));
#14979=CARTESIAN_POINT('Ctrl Pts',(0.679352081686668,-0.246942143572133,
-0.707917883896095));
#14980=CARTESIAN_POINT('Ctrl Pts',(0.663382628119203,-0.244251601209411,
-0.722929908501543));
#14981=CARTESIAN_POINT('Ctrl Pts',(0.631684198665438,-0.232861760990032,
-0.750785745543687));
#14982=CARTESIAN_POINT('Ctrl Pts',(0.615966552324775,-0.224161999508995,
-0.763642258217232));
#14983=CARTESIAN_POINT('Ctrl Pts',(0.587792702767295,-0.203463743702801,
-0.78555112003688));
#14984=CARTESIAN_POINT('Ctrl Pts',(0.573915184558107,-0.190326085855194,
-0.795684265985088));
#14985=CARTESIAN_POINT('Ctrl Pts',(0.548874290046456,-0.159766064500479,
-0.813159949759));
#14986=CARTESIAN_POINT('Ctrl Pts',(0.537715343527944,-0.142345102874864,
-0.820511285096538));
#14987=CARTESIAN_POINT('Ctrl Pts',(0.517157748491652,-0.099930567888331,
-0.833661031856294));
#14988=CARTESIAN_POINT('Ctrl Pts',(0.508899795931835,-0.0740444353928835,
-0.838633903678357));
#14989=CARTESIAN_POINT('Ctrl Pts',(0.504455939115715,-0.04763,-0.841298510752801));
#14990=CARTESIAN_POINT('Origin',(0.707106781186548,-0.04763,-0.707106781186547));
#14991=CARTESIAN_POINT('Origin',(0.,-0.166705,0.));
#14992=CARTESIAN_POINT('',(-0.980948,-0.28578,1.20131482833E-16));
#14993=CARTESIAN_POINT('Origin',(0.,-0.28578,0.));
#14994=CARTESIAN_POINT('',(-0.980948,-0.166705,1.20131482833E-16));
#14995=CARTESIAN_POINT('',(0.951592097314,-0.04763,0.238183666596899));
#14996=CARTESIAN_POINT('Origin',(0.,-0.04763,0.));
#14997=CARTESIAN_POINT('',(0.951592097314,-0.04763,-0.238183666596899));
#14998=CARTESIAN_POINT('Ctrl Pts',(0.951592097314,-0.04763,0.238183666596899));
#14999=CARTESIAN_POINT('Ctrl Pts',(0.952850216871763,-0.0740444353928835,
0.233157223576062));
#15000=CARTESIAN_POINT('Ctrl Pts',(0.955173119738174,-0.099930567888331,
0.223801617934945));
#15001=CARTESIAN_POINT('Ctrl Pts',(0.960411259488514,-0.142345102874864,
0.199966927975188));
#15002=CARTESIAN_POINT('Ctrl Pts',(0.963103647174702,-0.15976606450048,
0.1868781821531));
#15003=CARTESIAN_POINT('Ctrl Pts',(0.968453058988463,-0.190326085855194,
0.15681442133453));
#15004=CARTESIAN_POINT('Ctrl Pts',(0.971100730005489,-0.203463743702801,
0.139836317888042));
#15005=CARTESIAN_POINT('Ctrl Pts',(0.975530745318961,-0.224161999508995,
0.104422493053067));
#15006=CARTESIAN_POINT('Ctrl Pts',(0.977553872336861,-0.232861760990032,
0.0842175114474172));
#15007=CARTESIAN_POINT('Ctrl Pts',(0.980270995488453,-0.244251601209411,
0.0421062857595697));
#15008=CARTESIAN_POINT('Ctrl Pts',(0.980948,-0.246942143572133,0.0201990724523194));
#15009=CARTESIAN_POINT('Ctrl Pts',(0.980948,-0.246942143572133,-0.0201990724523194));
#15010=CARTESIAN_POINT('Ctrl Pts',(0.980270995488453,-0.244251601209411,
-0.0421062857595697));
#15011=CARTESIAN_POINT('Ctrl Pts',(0.977553872336861,-0.232861760990032,
-0.0842175114474172));
#15012=CARTESIAN_POINT('Ctrl Pts',(0.975530745318961,-0.224161999508995,
-0.104422493053067));
#15013=CARTESIAN_POINT('Ctrl Pts',(0.971100730005489,-0.203463743702801,
-0.139836317888042));
#15014=CARTESIAN_POINT('Ctrl Pts',(0.968453058988463,-0.190326085855194,
-0.15681442133453));
#15015=CARTESIAN_POINT('Ctrl Pts',(0.963103647174702,-0.15976606450048,
-0.1868781821531));
#15016=CARTESIAN_POINT('Ctrl Pts',(0.960411259488514,-0.142345102874864,
-0.199966927975188));
#15017=CARTESIAN_POINT('Ctrl Pts',(0.955173119738174,-0.099930567888331,
-0.223801617934945));
#15018=CARTESIAN_POINT('Ctrl Pts',(0.952850216871763,-0.0740444353928835,
-0.233157223576062));
#15019=CARTESIAN_POINT('Ctrl Pts',(0.951592097314,-0.0476299999999999,-0.238183666596899));
#15020=CARTESIAN_POINT('Origin',(0.,-0.04763,0.));
#15021=CARTESIAN_POINT('Origin',(0.,-0.04763,0.));
#15022=CARTESIAN_POINT('Origin',(1.,-0.04763,0.));
#15023=CARTESIAN_POINT('Origin',(1.,0.,0.));
#15024=CARTESIAN_POINT('Origin',(1.,-0.04763,0.));
#15025=CARTESIAN_POINT('Origin',(0.,-0.28578,0.));
#15026=CARTESIAN_POINT('Origin',(0.,-0.04763,0.));
#15027=CARTESIAN_POINT('',(0.,0.,0.));
#15028=CARTESIAN_POINT('Origin',(1.013815,0.445,0.));
#15029=CARTESIAN_POINT('',(-1.013815,0.445,-1.24156529467757E-16));
#15030=CARTESIAN_POINT('Origin',(0.,0.445,0.));
#15031=CARTESIAN_POINT('',(-0.991185,0.445,-1.21385153761287E-16));
#15032=CARTESIAN_POINT('Origin',(0.,0.445,0.));
#15033=CARTESIAN_POINT('Origin',(0.,0.4075,0.));
#15034=CARTESIAN_POINT('',(-1.013815,0.37,-1.24156529467757E-16));
#15035=CARTESIAN_POINT('Origin',(0.,0.37,0.));
#15036=CARTESIAN_POINT('',(-1.013815,0.4075,-1.24156529467757E-16));
#15037=CARTESIAN_POINT('Origin',(0.991185,0.37,0.));
#15038=CARTESIAN_POINT('',(-0.991185,0.37,-1.21385153761287E-16));
#15039=CARTESIAN_POINT('Origin',(0.,0.37,0.));
#15040=CARTESIAN_POINT('Origin',(0.,0.4075,0.));
#15041=CARTESIAN_POINT('',(-0.991185,0.4075,-1.21385153761287E-16));
#15042=CARTESIAN_POINT('Origin',(1.013815,-0.37,0.));
#15043=CARTESIAN_POINT('',(-1.013815,-0.37,-1.24156529467757E-16));
#15044=CARTESIAN_POINT('Origin',(0.,-0.37,0.));
#15045=CARTESIAN_POINT('',(-0.991185,-0.37,-1.21385153761287E-16));
#15046=CARTESIAN_POINT('Origin',(0.,-0.37,0.));
#15047=CARTESIAN_POINT('Origin',(0.,-0.4075,0.));
#15048=CARTESIAN_POINT('',(-1.013815,-0.445,-1.24156529467757E-16));
#15049=CARTESIAN_POINT('Origin',(0.,-0.445,0.));
#15050=CARTESIAN_POINT('',(-1.013815,-0.4075,-1.24156529467757E-16));
#15051=CARTESIAN_POINT('Origin',(0.991185,-0.445,0.));
#15052=CARTESIAN_POINT('',(-0.991185,-0.445,-1.21385153761287E-16));
#15053=CARTESIAN_POINT('Origin',(0.,-0.445,0.));
#15054=CARTESIAN_POINT('Origin',(0.,-0.4075,0.));
#15055=CARTESIAN_POINT('',(-0.991185,-0.4075,-1.21385153761287E-16));
#15056=CARTESIAN_POINT('',(0.,0.,0.));
#15057=CARTESIAN_POINT('',(0.,0.,0.));
#15058=CARTESIAN_POINT('',(0.,0.,0.));
#15059=CARTESIAN_POINT('',(0.,0.,0.));
#15060=CARTESIAN_POINT('',(0.,0.,0.));
#15061=CARTESIAN_POINT('',(0.,0.,0.));
#15062=CARTESIAN_POINT('Origin',(11.,0.,0.));
#15063=CARTESIAN_POINT('',(11.,7.34788079488412E-17,0.6));
#15064=CARTESIAN_POINT('Origin',(11.,0.,0.));
#15065=CARTESIAN_POINT('Origin',(0.05,0.,0.));
#15066=CARTESIAN_POINT('',(0.1,7.34788079488412E-17,0.6));
#15067=CARTESIAN_POINT('Origin',(0.1,0.,0.));
#15068=CARTESIAN_POINT('',(0.,-6.12323399573677E-17,0.5));
#15069=CARTESIAN_POINT('',(0.05,-6.73555739531044E-17,0.55));
#15070=CARTESIAN_POINT('Origin',(0.,0.,0.));
#15071=CARTESIAN_POINT('Origin',(0.,0.,0.));
#15072=CARTESIAN_POINT('',(0.,-7.34788079488412E-17,0.6));
#15073=CARTESIAN_POINT('Origin',(0.,0.,0.));
#15074=CARTESIAN_POINT('',(0.,0.,0.));
#15075=CARTESIAN_POINT('Origin',(0.0577350269189626,0.,-0.1));
#15076=CARTESIAN_POINT('',(0.0577350269189626,0.,-0.1));
#15077=CARTESIAN_POINT('',(0.115470053837925,0.,0.));
#15078=CARTESIAN_POINT('',(0.0934187836487032,0.,-0.0381939203391614));
#15079=CARTESIAN_POINT('',(0.0577350269189626,-0.2,-0.1));
#15080=CARTESIAN_POINT('',(0.0577350269189626,0.,-0.1));
#15081=CARTESIAN_POINT('',(0.115470053837925,-0.2,0.));
#15082=CARTESIAN_POINT('',(0.115470053837925,-0.2,0.));
#15083=CARTESIAN_POINT('',(0.115470053837925,0.,0.));
#15084=CARTESIAN_POINT('Origin',(-0.0577350269189626,0.,-0.1));
#15085=CARTESIAN_POINT('',(-0.0577350269189626,0.,-0.1));
#15086=CARTESIAN_POINT('',(0.0561324865405187,0.,-0.1));
#15087=CARTESIAN_POINT('',(-0.0577350269189626,-0.2,-0.1));
#15088=CARTESIAN_POINT('',(-0.0577350269189626,0.,-0.1));
#15089=CARTESIAN_POINT('',(0.0577350269189626,-0.2,-0.1));
#15090=CARTESIAN_POINT('Origin',(-0.115470053837925,0.,-1.38777878078145E-17));
#15091=CARTESIAN_POINT('',(-0.115470053837925,0.,-1.41410031829988E-17));
#15092=CARTESIAN_POINT('',(-0.0797862971081845,0.,-0.0618060796608387));
#15093=CARTESIAN_POINT('',(-0.115470053837925,-0.2,-1.38777878078145E-17));
#15094=CARTESIAN_POINT('',(-0.115470053837925,0.,-1.41410031829988E-17));
#15095=CARTESIAN_POINT('',(-0.0577350269189626,-0.2,-0.1));
#15096=CARTESIAN_POINT('Origin',(-0.0577350269189626,0.,0.1));
#15097=CARTESIAN_POINT('',(-0.0577350269189626,0.,0.1));
#15098=CARTESIAN_POINT('',(-0.0509187836487033,0.,0.111806079660839));
#15099=CARTESIAN_POINT('',(-0.0577350269189626,-0.2,0.1));
#15100=CARTESIAN_POINT('',(-0.0577350269189626,0.,0.1));
#15101=CARTESIAN_POINT('',(-0.115470053837925,-0.2,-1.41410031829988E-17));
#15102=CARTESIAN_POINT('Origin',(0.0577350269189626,0.,0.1));
#15103=CARTESIAN_POINT('',(0.0577350269189626,0.,0.1));
#15104=CARTESIAN_POINT('',(0.113867513459481,0.,0.1));
#15105=CARTESIAN_POINT('',(0.0577350269189626,-0.2,0.1));
#15106=CARTESIAN_POINT('',(0.0577350269189626,0.,0.1));
#15107=CARTESIAN_POINT('',(-0.0577350269189626,-0.2,0.1));
#15108=CARTESIAN_POINT('Origin',(0.115470053837925,0.,0.));
#15109=CARTESIAN_POINT('',(0.122286297108185,0.,-0.0118060796608386));
#15110=CARTESIAN_POINT('',(0.0577350269189626,-0.2,0.1));
#15111=CARTESIAN_POINT('Origin',(0.,-0.2,0.));
#15112=CARTESIAN_POINT('Origin',(0.17,0.,0.));
#15113=CARTESIAN_POINT('',(-0.17,-8.67361737988404E-18,-2.0818995585505E-17));
#15114=CARTESIAN_POINT('Origin',(0.,0.,0.));
#15115=CARTESIAN_POINT('Origin',(0.,-0.015,0.));
#15116=CARTESIAN_POINT('',(-0.1954,-0.0254,-2.39295984553393E-17));
#15117=CARTESIAN_POINT('Origin',(0.,-0.0254,0.));
#15118=CARTESIAN_POINT('',(-0.185,-0.015,-2.2655965784226E-17));
#15119=CARTESIAN_POINT('Origin',(0.,-0.2775,0.));
#15120=CARTESIAN_POINT('',(-0.1954,-0.5296,2.39295984553393E-17));
#15121=CARTESIAN_POINT('Origin',(0.,-0.5296,0.));
#15122=CARTESIAN_POINT('',(-0.1954,-0.2775,-2.39295984553393E-17));
#15123=CARTESIAN_POINT('Origin',(0.,-0.5625,0.));
#15124=CARTESIAN_POINT('',(-0.125,-0.6,-1.53080849893419E-17));
#15125=CARTESIAN_POINT('Origin',(0.,-0.6,0.));
#15126=CARTESIAN_POINT('',(-0.1625,-0.5625,-1.99005104861445E-17));
#15127=CARTESIAN_POINT('Origin',(0.,-0.6,0.));
#15128=CARTESIAN_POINT('',(0.,0.,0.));
#15129=CARTESIAN_POINT('',(0.,0.,0.));
#15130=CARTESIAN_POINT('Origin',(4.,0.,4.7));
#15131=CARTESIAN_POINT('',(3.75,-3.06161699786838E-17,4.8));
#15132=CARTESIAN_POINT('Origin',(4.,0.,4.8));
#15133=CARTESIAN_POINT('',(3.75,3.06161699786838E-17,5.6));
#15134=CARTESIAN_POINT('',(3.75,-3.06161699786838E-17,4.7));
#15135=CARTESIAN_POINT('Origin',(4.,0.,5.6));
#15136=CARTESIAN_POINT('Origin',(0.,2.,4.7));
#15137=CARTESIAN_POINT('',(-0.25,2.,4.8));
#15138=CARTESIAN_POINT('Origin',(0.,2.,4.8));
#15139=CARTESIAN_POINT('',(-0.25,2.,5.6));
#15140=CARTESIAN_POINT('',(-0.25,2.,4.7));
#15141=CARTESIAN_POINT('Origin',(0.,2.,5.6));
#15142=CARTESIAN_POINT('Origin',(-2.5,-2.5,4.7));
#15143=CARTESIAN_POINT('',(-2.725,-2.5,4.8));
#15144=CARTESIAN_POINT('Origin',(-2.5,-2.5,4.8));
#15145=CARTESIAN_POINT('',(-2.725,-2.5,5.6));
#15146=CARTESIAN_POINT('',(-2.725,-2.5,4.7));
#15147=CARTESIAN_POINT('Origin',(-2.5,-2.5,5.6));
#15148=CARTESIAN_POINT('Origin',(-2.5,-2.5,4.8));
#15149=CARTESIAN_POINT('',(-2.41196534727688,-1.70485856609033,4.8));
#15150=CARTESIAN_POINT('',(-2.41196534727688,-1.70485856609033,5.6));
#15151=CARTESIAN_POINT('',(-2.41196534727688,-1.70485856609033,4.8));
#15152=CARTESIAN_POINT('',(-1.70485856609033,-2.41196534727688,4.8));
#15153=CARTESIAN_POINT('Origin',(-2.5,-2.5,4.8));
#15154=CARTESIAN_POINT('',(-1.70485856609033,-2.41196534727688,5.6));
#15155=CARTESIAN_POINT('',(-1.70485856609033,-2.41196534727688,4.8));
#15156=CARTESIAN_POINT('Origin',(-2.5,-2.5,5.6));
#15157=CARTESIAN_POINT('Origin',(-0.353553390593274,0.353553390593274,4.8));
#15158=CARTESIAN_POINT('',(-0.965925826289068,-0.25881904510252,5.6));
#15159=CARTESIAN_POINT('',(-2.85355339059327,-2.14644660940673,5.6));
#15160=CARTESIAN_POINT('',(-0.965925826289068,-0.258819045102521,4.8));
#15161=CARTESIAN_POINT('',(-0.965925826289068,-0.258819045102521,4.8));
#15162=CARTESIAN_POINT('',(-2.85355339059327,-2.14644660940673,4.8));
#15163=CARTESIAN_POINT('Origin',(0.,0.,5.6));
#15164=CARTESIAN_POINT('',(-0.258819045102521,-0.965925826289068,5.6));
#15165=CARTESIAN_POINT('',(0.353553390593274,-0.353553390593274,5.6));
#15166=CARTESIAN_POINT('',(0.866025403784439,-0.5,5.6));
#15167=CARTESIAN_POINT('Origin',(0.,0.,5.6));
#15168=CARTESIAN_POINT('',(3.37550020016016,-0.5,5.6));
#15169=CARTESIAN_POINT('',(4.,-0.5,5.6));
#15170=CARTESIAN_POINT('',(3.37550020016016,0.5,5.6));
#15171=CARTESIAN_POINT('Origin',(4.,0.,5.6));
#15172=CARTESIAN_POINT('',(0.866025403784439,0.5,5.6));
#15173=CARTESIAN_POINT('',(0.,0.5,5.6));
#15174=CARTESIAN_POINT('',(0.5,0.866025403784439,5.6));
#15175=CARTESIAN_POINT('Origin',(0.,0.,5.6));
#15176=CARTESIAN_POINT('',(0.5,1.37550020016016,5.6));
#15177=CARTESIAN_POINT('',(0.5,2.,5.6));
#15178=CARTESIAN_POINT('',(-0.5,1.37550020016016,5.6));
#15179=CARTESIAN_POINT('Origin',(0.,2.,5.6));
#15180=CARTESIAN_POINT('',(-0.5,0.866025403784439,5.6));
#15181=CARTESIAN_POINT('',(-0.5,0.,5.6));
#15182=CARTESIAN_POINT('Origin',(0.,0.,5.6));
#15183=CARTESIAN_POINT('Origin',(-2.14644660940673,-2.85355339059327,4.8));
#15184=CARTESIAN_POINT('',(-0.25881904510252,-0.965925826289068,4.8));
#15185=CARTESIAN_POINT('',(0.353553390593274,-0.353553390593274,4.8));
#15186=CARTESIAN_POINT('',(-0.25881904510252,-0.965925826289068,4.8));
#15187=CARTESIAN_POINT('Origin',(0.,0.,4.8));
#15188=CARTESIAN_POINT('',(-0.5,0.866025403784439,4.8));
#15189=CARTESIAN_POINT('',(-0.5,0.866025403784439,4.8));
#15190=CARTESIAN_POINT('Origin',(0.,0.,4.8));
#15191=CARTESIAN_POINT('Origin',(0.,0.,4.8));
#15192=CARTESIAN_POINT('',(0.866025403784439,-0.5,4.8));
#15193=CARTESIAN_POINT('Origin',(0.,0.,4.8));
#15194=CARTESIAN_POINT('',(0.866025403784439,-0.5,4.8));
#15195=CARTESIAN_POINT('Origin',(4.,0.,4.8));
#15196=CARTESIAN_POINT('',(3.37550020016016,0.5,4.8));
#15197=CARTESIAN_POINT('',(3.37550020016016,0.5,4.8));
#15198=CARTESIAN_POINT('',(3.37550020016016,-0.5,4.8));
#15199=CARTESIAN_POINT('',(3.37550020016016,-0.5,4.8));
#15200=CARTESIAN_POINT('Origin',(4.,0.,4.8));
#15201=CARTESIAN_POINT('Origin',(4.,0.5,4.8));
#15202=CARTESIAN_POINT('',(0.866025403784439,0.5,4.8));
#15203=CARTESIAN_POINT('',(0.,0.5,4.8));
#15204=CARTESIAN_POINT('',(0.866025403784439,0.5,4.8));
#15205=CARTESIAN_POINT('Origin',(0.,0.,4.8));
#15206=CARTESIAN_POINT('',(-0.5,1.37550020016016,4.8));
#15207=CARTESIAN_POINT('',(-0.5,0.,4.8));
#15208=CARTESIAN_POINT('',(0.5,1.37550020016016,4.8));
#15209=CARTESIAN_POINT('Origin',(0.,2.,4.8));
#15210=CARTESIAN_POINT('',(0.5,0.866025403784439,4.8));
#15211=CARTESIAN_POINT('',(0.5,2.,4.8));
#15212=CARTESIAN_POINT('Origin',(0.,0.,4.8));
#15213=CARTESIAN_POINT('',(4.,-0.5,4.8));
#15214=CARTESIAN_POINT('',(-0.7,-8.57252759403147E-17,4.8));
#15215=CARTESIAN_POINT('Origin',(0.,0.,4.8));
#15216=CARTESIAN_POINT('Origin',(0.,-0.5,4.8));
#15217=CARTESIAN_POINT('Origin',(0.,2.,4.8));
#15218=CARTESIAN_POINT('',(0.5,1.37550020016016,4.8));
#15219=CARTESIAN_POINT('',(-0.5,1.37550020016016,4.8));
#15220=CARTESIAN_POINT('Origin',(0.5,0.,4.8));
#15221=CARTESIAN_POINT('',(0.5,0.866025403784439,4.8));
#15222=CARTESIAN_POINT('Origin',(-0.5,2.,4.8));
#15223=CARTESIAN_POINT('Origin',(0.,0.,4.8));
#15224=CARTESIAN_POINT('Origin',(0.,0.,2.95));
#15225=CARTESIAN_POINT('',(-0.7,-8.57252759403147E-17,2.95));
#15226=CARTESIAN_POINT('Origin',(0.,0.,2.95));
#15227=CARTESIAN_POINT('',(-0.5,6.12323399573677E-17,2.95));
#15228=CARTESIAN_POINT('Origin',(0.,0.,2.95));
#15229=CARTESIAN_POINT('Origin',(0.,0.,2.95));
#15230=CARTESIAN_POINT('',(-0.7,-8.57252759403147E-17,2.95));
#15231=CARTESIAN_POINT('Origin',(0.,0.,1.));
#15232=CARTESIAN_POINT('',(-0.5,-6.12323399573677E-17,1.));
#15233=CARTESIAN_POINT('',(-0.5,-6.12323399573677E-17,1.));
#15234=CARTESIAN_POINT('Origin',(0.,0.,1.));
#15235=CARTESIAN_POINT('Origin',(0.,0.,1.));
#15236=CARTESIAN_POINT('',(0.,0.,0.));
#15237=CARTESIAN_POINT('Origin',(-2.5,-2.5,5.5));
#15238=CARTESIAN_POINT('',(-2.665,-2.5,5.6));
#15239=CARTESIAN_POINT('Origin',(-2.5,-2.5,5.6));
#15240=CARTESIAN_POINT('',(-2.665,-2.5,6.7));
#15241=CARTESIAN_POINT('',(-2.665,-2.5,5.5));
#15242=CARTESIAN_POINT('Origin',(-2.5,-2.5,6.7));
#15243=CARTESIAN_POINT('Origin',(-2.5,-2.5,6.7));
#15244=CARTESIAN_POINT('Origin',(-2.5,-2.5,5.6));
#15245=CARTESIAN_POINT('',(-3.1,-2.5,8.1));
#15246=CARTESIAN_POINT('Origin',(-2.5,-2.5,8.1));
#15247=CARTESIAN_POINT('',(-3.1,-2.5,5.6));
#15248=CARTESIAN_POINT('',(-3.1,-2.5,5.6));
#15249=CARTESIAN_POINT('Origin',(-2.5,-2.5,5.6));
#15250=CARTESIAN_POINT('Origin',(-2.5,-2.5,8.1));
#15251=CARTESIAN_POINT('Origin',(-2.5,-2.5,5.6));
#15252=CARTESIAN_POINT('',(0.,0.,0.));
#15253=CARTESIAN_POINT('Origin',(0.,0.,1.8));
#15254=CARTESIAN_POINT('',(-0.505,-6.18446633569413E-17,2.05));
#15255=CARTESIAN_POINT('Origin',(0.,0.,2.05));
#15256=CARTESIAN_POINT('',(-0.505,-6.18446633569413E-17,1.8));
#15257=CARTESIAN_POINT('',(-0.505,-6.18446633569413E-17,1.8));
#15258=CARTESIAN_POINT('Origin',(0.,0.,1.8));
#15259=CARTESIAN_POINT('Origin',(0.,0.,1.8));
#15260=CARTESIAN_POINT('',(-0.7,-8.57252759403147E-17,2.05));
#15261=CARTESIAN_POINT('Origin',(0.,0.,2.05));
#15262=CARTESIAN_POINT('',(-0.7,-8.57252759403147E-17,1.8));
#15263=CARTESIAN_POINT('',(-0.7,-8.57252759403147E-17,1.8));
#15264=CARTESIAN_POINT('Origin',(0.,0.,1.8));
#15265=CARTESIAN_POINT('Origin',(0.,0.,2.05));
#15266=CARTESIAN_POINT('Origin',(0.,0.,1.8));
#15267=CARTESIAN_POINT('',(0.,0.,0.));
#15268=CARTESIAN_POINT('Origin',(0.49,0.,1.4));
#15269=CARTESIAN_POINT('',(0.49,0.122167917228706,1.28909463493591));
#15270=CARTESIAN_POINT('',(0.49,0.122167917228706,1.51090536506409));
#15271=CARTESIAN_POINT('',(0.49,0.122167917228706,1.));
#15272=CARTESIAN_POINT('Origin',(0.49,0.,1.4));
#15273=CARTESIAN_POINT('Origin',(0.49,0.,1.4));
#15274=CARTESIAN_POINT('',(0.49,-0.122167917228706,1.28909463493591));
#15275=CARTESIAN_POINT('Ctrl Pts',(0.49,-0.122167917228706,1.28909463493591));
#15276=CARTESIAN_POINT('Ctrl Pts',(0.490448531679987,-0.120368913626296,
1.28711294069536));
#15277=CARTESIAN_POINT('Ctrl Pts',(0.490895245371685,-0.118534896565231,
1.28518965877367));
#15278=CARTESIAN_POINT('Ctrl Pts',(0.494795015531646,-0.102111993019358,
1.2687667552278));
#15279=CARTESIAN_POINT('Ctrl Pts',(0.498442514607594,-0.0836597150224318,
1.25609154388858));
#15280=CARTESIAN_POINT('Ctrl Pts',(0.50357781976106,-0.0430495960471595,
1.23920409039234));
#15281=CARTESIAN_POINT('Ctrl Pts',(0.505,-0.020880094330741,1.235));
#15282=CARTESIAN_POINT('Ctrl Pts',(0.505,0.020880094330741,1.235));
#15283=CARTESIAN_POINT('Ctrl Pts',(0.50357781976106,0.0430495960471595,
1.23920409039234));
#15284=CARTESIAN_POINT('Ctrl Pts',(0.498442514607594,0.0836597150224318,
1.25609154388858));
#15285=CARTESIAN_POINT('Ctrl Pts',(0.494795015531646,0.102111993019358,
1.2687667552278));
#15286=CARTESIAN_POINT('Ctrl Pts',(0.490895245371684,0.118534896565231,
1.28518965877367));
#15287=CARTESIAN_POINT('Ctrl Pts',(0.490448531679987,0.120368913626296,
1.28711294069536));
#15288=CARTESIAN_POINT('Ctrl Pts',(0.49,0.122167917228706,1.28909463493591));
#15289=CARTESIAN_POINT('',(0.49,-0.122167917228706,1.51090536506409));
#15290=CARTESIAN_POINT('Origin',(0.49,0.,1.4));
#15291=CARTESIAN_POINT('',(0.505,-1.70422299968729E-17,1.565));
#15292=CARTESIAN_POINT('Ctrl Pts',(0.505,-6.93889390390723E-18,1.565));
#15293=CARTESIAN_POINT('Ctrl Pts',(0.505,-0.020880094330741,1.565));
#15294=CARTESIAN_POINT('Ctrl Pts',(0.50357781976106,-0.0430495960471595,
1.56079590960766));
#15295=CARTESIAN_POINT('Ctrl Pts',(0.498442514607594,-0.0836597150224318,
1.54390845611142));
#15296=CARTESIAN_POINT('Ctrl Pts',(0.494795015531646,-0.102111993019358,
1.5312332447722));
#15297=CARTESIAN_POINT('Ctrl Pts',(0.490895245371684,-0.118534896565231,
1.51481034122633));
#15298=CARTESIAN_POINT('Ctrl Pts',(0.490448531679987,-0.120368913626296,
1.51288705930464));
#15299=CARTESIAN_POINT('Ctrl Pts',(0.49,-0.122167917228706,1.51090536506409));
#15300=CARTESIAN_POINT('',(0.9,-2.02066721859313E-17,1.565));
#15301=CARTESIAN_POINT('',(0.49,-2.02066721859313E-17,1.565));
#15302=CARTESIAN_POINT('',(0.884745726183518,0.165,1.4));
#15303=CARTESIAN_POINT('Ctrl Pts',(0.884745726183518,0.165,1.4));
#15304=CARTESIAN_POINT('Ctrl Pts',(0.884745726183518,0.165,1.37923124059256));
#15305=CARTESIAN_POINT('Ctrl Pts',(0.885552759505264,0.160839719007584,
1.35711110492666));
#15306=CARTESIAN_POINT('Ctrl Pts',(0.888448648150043,0.143986470216691,
1.31647293736623));
#15307=CARTESIAN_POINT('Ctrl Pts',(0.890493604851638,0.131295993814186,
1.29795075602263));
#15308=CARTESIAN_POINT('Ctrl Pts',(0.89431723432394,0.102049819008125,1.26870458121656));
#15309=CARTESIAN_POINT('Ctrl Pts',(0.896347088899543,0.0835273920906824,
1.25601365401642));
#15310=CARTESIAN_POINT('Ctrl Pts',(0.899208271860583,0.0428883760934127,
1.23916007816136));
#15311=CARTESIAN_POINT('Ctrl Pts',(0.9,0.0207679427235068,1.235));
#15312=CARTESIAN_POINT('Ctrl Pts',(0.9,-0.0207679427235068,1.235));
#15313=CARTESIAN_POINT('Ctrl Pts',(0.899208271860583,-0.0428883760934127,
1.23916007816136));
#15314=CARTESIAN_POINT('Ctrl Pts',(0.896347088899543,-0.0835273920906823,
1.25601365401642));
#15315=CARTESIAN_POINT('Ctrl Pts',(0.89431723432394,-0.102049819008125,
1.26870458121656));
#15316=CARTESIAN_POINT('Ctrl Pts',(0.890493604851638,-0.131295993814186,
1.29795075602263));
#15317=CARTESIAN_POINT('Ctrl Pts',(0.888448648150043,-0.143986470216691,
1.31647293736623));
#15318=CARTESIAN_POINT('Ctrl Pts',(0.885552759505264,-0.160839719007584,
1.35711110492666));
#15319=CARTESIAN_POINT('Ctrl Pts',(0.884745726183518,-0.165,1.37923124059256));
#15320=CARTESIAN_POINT('Ctrl Pts',(0.884745726183518,-0.165,1.42076875940744));
#15321=CARTESIAN_POINT('Ctrl Pts',(0.885552759505264,-0.160839719007584,
1.44288889507334));
#15322=CARTESIAN_POINT('Ctrl Pts',(0.888448648150043,-0.14398647021669,
1.48352706263377));
#15323=CARTESIAN_POINT('Ctrl Pts',(0.890493604851638,-0.131295993814186,
1.50204924397737));
#15324=CARTESIAN_POINT('Ctrl Pts',(0.89431723432394,-0.102049819008125,
1.53129541878344));
#15325=CARTESIAN_POINT('Ctrl Pts',(0.896347088899543,-0.0835273920906824,
1.54398634598358));
#15326=CARTESIAN_POINT('Ctrl Pts',(0.899208271860583,-0.0428883760934128,
1.56083992183864));
#15327=CARTESIAN_POINT('Ctrl Pts',(0.9,-0.0207679427235068,1.565));
#15328=CARTESIAN_POINT('Ctrl Pts',(0.9,-6.93889390390723E-18,1.565));
#15329=CARTESIAN_POINT('Ctrl Pts',(0.9,-3.46944695195361E-17,1.565));
#15330=CARTESIAN_POINT('Ctrl Pts',(0.9,0.0207679427235068,1.565));
#15331=CARTESIAN_POINT('Ctrl Pts',(0.899208271860583,0.0428883760934127,
1.56083992183864));
#15332=CARTESIAN_POINT('Ctrl Pts',(0.896347088899543,0.0835273920906824,
1.54398634598358));
#15333=CARTESIAN_POINT('Ctrl Pts',(0.89431723432394,0.102049819008125,1.53129541878344));
#15334=CARTESIAN_POINT('Ctrl Pts',(0.890493604851638,0.131295993814186,
1.50204924397737));
#15335=CARTESIAN_POINT('Ctrl Pts',(0.888448648150043,0.143986470216691,
1.48352706263377));
#15336=CARTESIAN_POINT('Ctrl Pts',(0.885552759505264,0.160839719007584,
1.44288889507334));
#15337=CARTESIAN_POINT('Ctrl Pts',(0.884745726183518,0.165,1.42076875940744));
#15338=CARTESIAN_POINT('Ctrl Pts',(0.884745726183518,0.165,1.4));
#15339=CARTESIAN_POINT('Ctrl Pts',(0.49,0.122167917228706,1.51090536506409));
#15340=CARTESIAN_POINT('Ctrl Pts',(0.490448531679987,0.120368913626296,
1.51288705930464));
#15341=CARTESIAN_POINT('Ctrl Pts',(0.490895245371685,0.118534896565231,
1.51481034122633));
#15342=CARTESIAN_POINT('Ctrl Pts',(0.494795015531646,0.102111993019358,
1.5312332447722));
#15343=CARTESIAN_POINT('Ctrl Pts',(0.498442514607594,0.0836597150224318,
1.54390845611142));
#15344=CARTESIAN_POINT('Ctrl Pts',(0.50357781976106,0.0430495960471594,
1.56079590960766));
#15345=CARTESIAN_POINT('Ctrl Pts',(0.505,0.020880094330741,1.565));
#15346=CARTESIAN_POINT('Ctrl Pts',(0.505,0.,1.565));
#15347=CARTESIAN_POINT('Origin',(0.49,0.,1.4));
#15348=CARTESIAN_POINT('',(0.49,-0.122167917228706,1.));
#15349=CARTESIAN_POINT('Origin',(0.,0.,1.));
#15350=CARTESIAN_POINT('',(-0.505,-6.18446633569413E-17,1.8));
#15351=CARTESIAN_POINT('Origin',(0.,0.,1.8));
#15352=CARTESIAN_POINT('',(-0.505,-6.18446633569413E-17,1.));
#15353=CARTESIAN_POINT('',(-0.505,-6.18446633569413E-17,1.));
#15354=CARTESIAN_POINT('Origin',(0.,0.,1.));
#15355=CARTESIAN_POINT('Origin',(0.,0.,1.));
#15356=CARTESIAN_POINT('',(-0.9,-1.10218211923262E-16,1.8));
#15357=CARTESIAN_POINT('Origin',(0.,0.,1.8));
#15358=CARTESIAN_POINT('',(-0.9,-1.10218211923262E-16,1.));
#15359=CARTESIAN_POINT('',(-0.9,-1.10218211923262E-16,1.));
#15360=CARTESIAN_POINT('Origin',(0.,0.,1.));
#15361=CARTESIAN_POINT('Origin',(0.,0.,1.8));
#15362=CARTESIAN_POINT('Origin',(0.,0.,1.));
#15363=CARTESIAN_POINT('',(0.,0.,0.));
#15364=CARTESIAN_POINT('Origin',(0.,2.,9.1));
#15365=CARTESIAN_POINT('',(-0.165,2.,9.1));
#15366=CARTESIAN_POINT('Origin',(0.,2.,9.1));
#15367=CARTESIAN_POINT('',(-0.165,2.,10.1));
#15368=CARTESIAN_POINT('',(-0.165,2.,9.1));
#15369=CARTESIAN_POINT('Origin',(0.,2.,10.1));
#15370=CARTESIAN_POINT('Origin',(0.,2.,9.1));
#15371=CARTESIAN_POINT('Origin',(0.,2.,6.));
#15372=CARTESIAN_POINT('',(-0.7,2.,6.));
#15373=CARTESIAN_POINT('Origin',(0.,2.,6.));
#15374=CARTESIAN_POINT('',(-0.3,2.,6.));
#15375=CARTESIAN_POINT('Origin',(0.,2.,6.));
#15376=CARTESIAN_POINT('Origin',(0.,2.,5.6));
#15377=CARTESIAN_POINT('',(-0.7,2.,5.6));
#15378=CARTESIAN_POINT('Origin',(0.,2.,5.6));
#15379=CARTESIAN_POINT('',(-0.3,2.,5.6));
#15380=CARTESIAN_POINT('Origin',(0.,2.,5.6));
#15381=CARTESIAN_POINT('Origin',(0.,2.,5.6));
#15382=CARTESIAN_POINT('',(-0.7,2.,5.6));
#15383=CARTESIAN_POINT('Origin',(0.,2.,4.8));
#15384=CARTESIAN_POINT('',(-0.3,2.,4.8));
#15385=CARTESIAN_POINT('',(-0.3,2.,4.8));
#15386=CARTESIAN_POINT('Origin',(0.,2.,4.8));
#15387=CARTESIAN_POINT('Origin',(0.,2.,4.8));
#15388=CARTESIAN_POINT('',(-0.3,2.,10.1));
#15389=CARTESIAN_POINT('Origin',(0.,2.,10.1));
#15390=CARTESIAN_POINT('',(-0.3,2.,4.8));
#15391=CARTESIAN_POINT('Origin',(0.,2.,10.1));
#15392=CARTESIAN_POINT('Origin',(0.,2.,4.8));
#15393=CARTESIAN_POINT('',(0.,0.,0.));
#15394=CARTESIAN_POINT('Origin',(0.,2.,6.));
#15395=CARTESIAN_POINT('',(-0.305,2.,8.8));
#15396=CARTESIAN_POINT('Origin',(0.,2.,8.8));
#15397=CARTESIAN_POINT('',(-0.305,2.,6.));
#15398=CARTESIAN_POINT('',(-0.305,2.,6.));
#15399=CARTESIAN_POINT('Origin',(0.,2.,6.));
#15400=CARTESIAN_POINT('Origin',(0.,2.,6.));
#15401=CARTESIAN_POINT('',(-0.5,2.,8.8));
#15402=CARTESIAN_POINT('Origin',(0.,2.,8.8));
#15403=CARTESIAN_POINT('',(-0.5,2.,6.));
#15404=CARTESIAN_POINT('',(-0.5,2.,6.));
#15405=CARTESIAN_POINT('Origin',(0.,2.,6.));
#15406=CARTESIAN_POINT('Origin',(0.,2.,8.8));
#15407=CARTESIAN_POINT('Origin',(0.,2.,6.));
#15408=CARTESIAN_POINT('',(0.,0.,0.));
#15409=CARTESIAN_POINT('Origin',(0.,2.,9.6));
#15410=CARTESIAN_POINT('',(-0.305,2.,10.1));
#15411=CARTESIAN_POINT('Origin',(0.,2.,10.1));
#15412=CARTESIAN_POINT('',(-0.305,2.,9.6));
#15413=CARTESIAN_POINT('',(-0.305,2.,9.6));
#15414=CARTESIAN_POINT('Origin',(0.,2.,9.6));
#15415=CARTESIAN_POINT('Origin',(0.,2.,9.6));
#15416=CARTESIAN_POINT('',(-0.5,2.,10.1));
#15417=CARTESIAN_POINT('Origin',(0.,2.,10.1));
#15418=CARTESIAN_POINT('',(-0.5,2.,9.6));
#15419=CARTESIAN_POINT('',(-0.5,2.,9.6));
#15420=CARTESIAN_POINT('Origin',(0.,2.,9.6));
#15421=CARTESIAN_POINT('Origin',(0.,2.,10.1));
#15422=CARTESIAN_POINT('Origin',(0.,2.,9.6));
#15423=CARTESIAN_POINT('',(0.,0.,0.));
#15424=CARTESIAN_POINT('Origin',(0.,2.,10.1));
#15425=CARTESIAN_POINT('',(-0.225,2.,10.3));
#15426=CARTESIAN_POINT('Origin',(0.,2.,10.3));
#15427=CARTESIAN_POINT('',(-0.225,2.,10.1));
#15428=CARTESIAN_POINT('',(-0.225,2.,10.1));
#15429=CARTESIAN_POINT('Origin',(0.,2.,10.1));
#15430=CARTESIAN_POINT('Origin',(0.,2.,10.1));
#15431=CARTESIAN_POINT('',(-0.5,2.,10.3));
#15432=CARTESIAN_POINT('Origin',(0.,2.,10.3));
#15433=CARTESIAN_POINT('',(-0.5,2.,10.1));
#15434=CARTESIAN_POINT('',(-0.5,2.,10.1));
#15435=CARTESIAN_POINT('Origin',(0.,2.,10.1));
#15436=CARTESIAN_POINT('Origin',(0.,2.,10.3));
#15437=CARTESIAN_POINT('Origin',(0.,2.,10.1));
#15438=CARTESIAN_POINT('',(0.,0.,0.));
#15439=CARTESIAN_POINT('Origin',(4.,0.,7.1));
#15440=CARTESIAN_POINT('',(3.835,-2.02066721859313E-17,7.1));
#15441=CARTESIAN_POINT('Origin',(4.,0.,7.1));
#15442=CARTESIAN_POINT('',(3.835,2.02066721859313E-17,8.1));
#15443=CARTESIAN_POINT('',(3.835,-2.02066721859313E-17,7.1));
#15444=CARTESIAN_POINT('Origin',(4.,0.,8.1));
#15445=CARTESIAN_POINT('Origin',(4.,0.,7.1));
#15446=CARTESIAN_POINT('Origin',(4.,0.,6.));
#15447=CARTESIAN_POINT('',(3.3,-8.57252759403147E-17,6.));
#15448=CARTESIAN_POINT('Origin',(4.,0.,6.));
#15449=CARTESIAN_POINT('',(3.7,-3.67394039744206E-17,6.));
#15450=CARTESIAN_POINT('Origin',(4.,0.,6.));
#15451=CARTESIAN_POINT('Origin',(4.,0.,5.6));
#15452=CARTESIAN_POINT('',(3.3,-8.57252759403147E-17,5.6));
#15453=CARTESIAN_POINT('Origin',(4.,0.,5.6));
#15454=CARTESIAN_POINT('',(3.7,3.67394039744206E-17,5.6));
#15455=CARTESIAN_POINT('Origin',(4.,0.,5.6));
#15456=CARTESIAN_POINT('Origin',(4.,0.,5.6));
#15457=CARTESIAN_POINT('',(3.3,-8.57252759403147E-17,5.6));
#15458=CARTESIAN_POINT('Origin',(4.,0.,4.8));
#15459=CARTESIAN_POINT('',(3.7,-3.67394039744206E-17,4.8));
#15460=CARTESIAN_POINT('',(3.7,-3.67394039744206E-17,4.8));
#15461=CARTESIAN_POINT('Origin',(4.,0.,4.8));
#15462=CARTESIAN_POINT('Origin',(4.,0.,4.8));
#15463=CARTESIAN_POINT('',(3.7,-3.67394039744206E-17,8.1));
#15464=CARTESIAN_POINT('Origin',(4.,0.,8.1));
#15465=CARTESIAN_POINT('',(3.7,-3.67394039744206E-17,4.8));
#15466=CARTESIAN_POINT('Origin',(4.,0.,8.1));
#15467=CARTESIAN_POINT('Origin',(4.,0.,4.8));
#15468=CARTESIAN_POINT('',(0.,0.,0.));
#15469=CARTESIAN_POINT('Origin',(4.,0.,6.));
#15470=CARTESIAN_POINT('',(3.695,-3.73517273739942E-17,6.8));
#15471=CARTESIAN_POINT('Origin',(4.,0.,6.8));
#15472=CARTESIAN_POINT('',(3.695,-3.73517273739942E-17,6.));
#15473=CARTESIAN_POINT('',(3.695,-3.73517273739942E-17,6.));
#15474=CARTESIAN_POINT('Origin',(4.,0.,6.));
#15475=CARTESIAN_POINT('Origin',(4.,0.,6.));
#15476=CARTESIAN_POINT('',(3.5,-6.12323399573677E-17,6.8));
#15477=CARTESIAN_POINT('Origin',(4.,0.,6.8));
#15478=CARTESIAN_POINT('',(3.5,-6.12323399573677E-17,6.));
#15479=CARTESIAN_POINT('',(3.5,-6.12323399573677E-17,6.));
#15480=CARTESIAN_POINT('Origin',(4.,0.,6.));
#15481=CARTESIAN_POINT('Origin',(4.,0.,6.8));
#15482=CARTESIAN_POINT('Origin',(4.,0.,6.));
#15483=CARTESIAN_POINT('',(0.,0.,0.));
#15484=CARTESIAN_POINT('Origin',(4.,0.,7.6));
#15485=CARTESIAN_POINT('',(3.695,-3.73517273739942E-17,8.1));
#15486=CARTESIAN_POINT('Origin',(4.,0.,8.1));
#15487=CARTESIAN_POINT('',(3.695,-3.73517273739942E-17,7.6));
#15488=CARTESIAN_POINT('',(3.695,-3.73517273739942E-17,7.6));
#15489=CARTESIAN_POINT('Origin',(4.,0.,7.6));
#15490=CARTESIAN_POINT('Origin',(4.,0.,7.6));
#15491=CARTESIAN_POINT('',(3.5,-6.12323399573677E-17,8.1));
#15492=CARTESIAN_POINT('Origin',(4.,0.,8.1));
#15493=CARTESIAN_POINT('',(3.5,-6.12323399573677E-17,7.6));
#15494=CARTESIAN_POINT('',(3.5,-6.12323399573677E-17,7.6));
#15495=CARTESIAN_POINT('Origin',(4.,0.,7.6));
#15496=CARTESIAN_POINT('Origin',(4.,0.,8.1));
#15497=CARTESIAN_POINT('Origin',(4.,0.,7.6));
#15498=CARTESIAN_POINT('',(0.,0.,0.));
#15499=CARTESIAN_POINT('Origin',(4.,0.,8.1));
#15500=CARTESIAN_POINT('',(3.775,-2.75545529808154E-17,8.3));
#15501=CARTESIAN_POINT('Origin',(4.,0.,8.3));
#15502=CARTESIAN_POINT('',(3.775,-2.75545529808154E-17,8.1));
#15503=CARTESIAN_POINT('',(3.775,-2.75545529808154E-17,8.1));
#15504=CARTESIAN_POINT('Origin',(4.,0.,8.1));
#15505=CARTESIAN_POINT('Origin',(4.,0.,8.1));
#15506=CARTESIAN_POINT('',(3.5,-6.12323399573677E-17,8.3));
#15507=CARTESIAN_POINT('Origin',(4.,0.,8.3));
#15508=CARTESIAN_POINT('',(3.5,-6.12323399573677E-17,8.1));
#15509=CARTESIAN_POINT('',(3.5,-6.12323399573677E-17,8.1));
#15510=CARTESIAN_POINT('Origin',(4.,0.,8.1));
#15511=CARTESIAN_POINT('Origin',(4.,0.,8.3));
#15512=CARTESIAN_POINT('Origin',(4.,0.,8.1));
#15513=CARTESIAN_POINT('',(0.,0.,0.));
#15514=CARTESIAN_POINT('Origin',(0.3,0.4,0.));
#15515=CARTESIAN_POINT('',(-0.3,0.4,-3.67394039744206E-17));
#15516=CARTESIAN_POINT('Origin',(0.,0.4,0.));
#15517=CARTESIAN_POINT('Origin',(0.,0.375,0.));
#15518=CARTESIAN_POINT('',(-0.35,0.35,-4.28626379701573E-17));
#15519=CARTESIAN_POINT('Origin',(0.,0.35,0.));
#15520=CARTESIAN_POINT('',(-0.325,0.375,-3.9801020972289E-17));
#15521=CARTESIAN_POINT('Origin',(0.,0.19,0.));
#15522=CARTESIAN_POINT('',(-0.35,0.03,-4.28626379701574E-17));
#15523=CARTESIAN_POINT('Origin',(0.,0.03,0.));
#15524=CARTESIAN_POINT('',(-0.35,0.19,-4.28626379701574E-17));
#15525=CARTESIAN_POINT('Origin',(0.,0.0149999999999999,0.));
#15526=CARTESIAN_POINT('',(-0.32,-3.29597460435593E-17,-3.91886975727153E-17));
#15527=CARTESIAN_POINT('Origin',(0.,0.,0.));
#15528=CARTESIAN_POINT('',(-0.335,0.0149999999999999,-4.10256677714363E-17));
#15529=CARTESIAN_POINT('Origin',(0.22,0.,0.));
#15530=CARTESIAN_POINT('',(-0.22,-6.93889390390723E-18,-2.69422295812418E-17));
#15531=CARTESIAN_POINT('Origin',(0.,0.,0.));
#15532=CARTESIAN_POINT('Origin',(0.,-0.02,0.));
#15533=CARTESIAN_POINT('',(-0.1954,-0.0492,2.39295984553393E-17));
#15534=CARTESIAN_POINT('Origin',(0.,-0.0492,0.));
#15535=CARTESIAN_POINT('',(-0.21,-0.02,-2.57175827820944E-17));
#15536=CARTESIAN_POINT('Origin',(0.,-0.8,0.));
#15537=CARTESIAN_POINT('',(-0.1954,-1.5646,2.39295984553393E-17));
#15538=CARTESIAN_POINT('Origin',(0.,-1.5646,0.));
#15539=CARTESIAN_POINT('',(-0.1954,-0.8,-2.39295984553393E-17));
#15540=CARTESIAN_POINT('Origin',(0.,-1.58,0.));
#15541=CARTESIAN_POINT('',(-0.16,-1.6,-1.95943487863577E-17));
#15542=CARTESIAN_POINT('Origin',(0.,-1.6,0.));
#15543=CARTESIAN_POINT('',(-0.18,-1.58,-2.20436423846524E-17));
#15544=CARTESIAN_POINT('Origin',(0.,-1.6,0.));
#15545=CARTESIAN_POINT('Origin',(0.0866025403784439,-0.4,-0.15));
#15546=CARTESIAN_POINT('',(0.173205080756888,-0.4,0.));
#15547=CARTESIAN_POINT('',(0.0866025403784439,-0.4,-0.15));
#15548=CARTESIAN_POINT('',(0.173205080756888,-0.4,0.));
#15549=CARTESIAN_POINT('',(0.0866025403784439,-0.64,-0.15));
#15550=CARTESIAN_POINT('',(0.0866025403784439,-0.4,-0.15));
#15551=CARTESIAN_POINT('',(0.173205080756888,-0.64,0.));
#15552=CARTESIAN_POINT('',(0.173205080756888,-0.64,0.));
#15553=CARTESIAN_POINT('',(0.173205080756888,-0.4,0.));
#15554=CARTESIAN_POINT('Origin',(-0.0866025403784438,-0.4,-0.15));
#15555=CARTESIAN_POINT('',(-0.0866025403784438,-0.4,-0.15));
#15556=CARTESIAN_POINT('',(0.0866025403784439,-0.4,-0.15));
#15557=CARTESIAN_POINT('',(-0.0866025403784438,-0.64,-0.15));
#15558=CARTESIAN_POINT('',(-0.0866025403784438,-0.4,-0.15));
#15559=CARTESIAN_POINT('',(0.0866025403784439,-0.64,-0.15));
#15560=CARTESIAN_POINT('Origin',(-0.173205080756888,-0.4,-2.77555756156289E-17));
#15561=CARTESIAN_POINT('',(-0.173205080756888,-0.4,-2.12115047744981E-17));
#15562=CARTESIAN_POINT('',(-0.0866025403784438,-0.4,-0.15));
#15563=CARTESIAN_POINT('',(-0.173205080756888,-0.64,-2.77555756156289E-17));
#15564=CARTESIAN_POINT('',(-0.173205080756888,-0.4,-2.12115047744981E-17));
#15565=CARTESIAN_POINT('',(-0.0866025403784438,-0.64,-0.15));
#15566=CARTESIAN_POINT('Origin',(-0.0866025403784439,-0.4,0.15));
#15567=CARTESIAN_POINT('',(-0.0866025403784439,-0.4,0.15));
#15568=CARTESIAN_POINT('',(-0.173205080756888,-0.4,-2.12115047744981E-17));
#15569=CARTESIAN_POINT('',(-0.0866025403784439,-0.64,0.15));
#15570=CARTESIAN_POINT('',(-0.0866025403784439,-0.4,0.15));
#15571=CARTESIAN_POINT('',(-0.173205080756888,-0.64,-2.12115047744981E-17));
#15572=CARTESIAN_POINT('Origin',(0.0866025403784439,-0.4,0.15));
#15573=CARTESIAN_POINT('',(0.0866025403784439,-0.4,0.15));
#15574=CARTESIAN_POINT('',(-0.0866025403784439,-0.4,0.15));
#15575=CARTESIAN_POINT('',(0.0866025403784439,-0.64,0.15));
#15576=CARTESIAN_POINT('',(0.0866025403784439,-0.4,0.15));
#15577=CARTESIAN_POINT('',(-0.0866025403784439,-0.64,0.15));
#15578=CARTESIAN_POINT('Origin',(0.173205080756888,-0.4,0.));
#15579=CARTESIAN_POINT('',(0.0866025403784439,-0.4,0.15));
#15580=CARTESIAN_POINT('',(0.0866025403784439,-0.64,0.15));
#15581=CARTESIAN_POINT('Origin',(0.,-0.4,-2.77555756156289E-17));
#15582=CARTESIAN_POINT('Origin',(0.,-0.64,-2.77555756156289E-17));
#15583=CARTESIAN_POINT('',(0.,0.,0.));
#15584=CARTESIAN_POINT('Origin',(0.,-0.4,0.));
#15585=CARTESIAN_POINT('',(-0.1954,-0.4,2.39295984553393E-17));
#15586=CARTESIAN_POINT('Origin',(0.,-0.4,0.));
#15587=CARTESIAN_POINT('Origin',(0.0577350269189626,0.,-0.1));
#15588=CARTESIAN_POINT('',(0.0577350269189626,0.,-0.1));
#15589=CARTESIAN_POINT('',(0.115470053837925,0.,0.));
#15590=CARTESIAN_POINT('',(0.0934187836487032,0.,-0.0381939203391614));
#15591=CARTESIAN_POINT('',(0.0577350269189626,-0.2,-0.1));
#15592=CARTESIAN_POINT('',(0.0577350269189626,0.,-0.1));
#15593=CARTESIAN_POINT('',(0.115470053837925,-0.2,0.));
#15594=CARTESIAN_POINT('',(0.115470053837925,-0.2,0.));
#15595=CARTESIAN_POINT('',(0.115470053837925,0.,0.));
#15596=CARTESIAN_POINT('Origin',(-0.0577350269189626,0.,-0.1));
#15597=CARTESIAN_POINT('',(-0.0577350269189626,0.,-0.1));
#15598=CARTESIAN_POINT('',(0.0561324865405187,0.,-0.1));
#15599=CARTESIAN_POINT('',(-0.0577350269189626,-0.2,-0.1));
#15600=CARTESIAN_POINT('',(-0.0577350269189626,0.,-0.1));
#15601=CARTESIAN_POINT('',(0.0577350269189626,-0.2,-0.1));
#15602=CARTESIAN_POINT('Origin',(-0.115470053837925,0.,-1.38777878078145E-17));
#15603=CARTESIAN_POINT('',(-0.115470053837925,0.,-1.41410031829988E-17));
#15604=CARTESIAN_POINT('',(-0.0797862971081845,0.,-0.0618060796608387));
#15605=CARTESIAN_POINT('',(-0.115470053837925,-0.2,-1.38777878078145E-17));
#15606=CARTESIAN_POINT('',(-0.115470053837925,0.,-1.41410031829988E-17));
#15607=CARTESIAN_POINT('',(-0.0577350269189626,-0.2,-0.1));
#15608=CARTESIAN_POINT('Origin',(-0.0577350269189626,0.,0.1));
#15609=CARTESIAN_POINT('',(-0.0577350269189626,0.,0.1));
#15610=CARTESIAN_POINT('',(-0.0509187836487033,0.,0.111806079660839));
#15611=CARTESIAN_POINT('',(-0.0577350269189626,-0.2,0.1));
#15612=CARTESIAN_POINT('',(-0.0577350269189626,0.,0.1));
#15613=CARTESIAN_POINT('',(-0.115470053837925,-0.2,-1.41410031829988E-17));
#15614=CARTESIAN_POINT('Origin',(0.0577350269189626,0.,0.1));
#15615=CARTESIAN_POINT('',(0.0577350269189626,0.,0.1));
#15616=CARTESIAN_POINT('',(0.113867513459481,0.,0.1));
#15617=CARTESIAN_POINT('',(0.0577350269189626,-0.2,0.1));
#15618=CARTESIAN_POINT('',(0.0577350269189626,0.,0.1));
#15619=CARTESIAN_POINT('',(-0.0577350269189626,-0.2,0.1));
#15620=CARTESIAN_POINT('Origin',(0.115470053837925,0.,0.));
#15621=CARTESIAN_POINT('',(0.122286297108185,0.,-0.0118060796608386));
#15622=CARTESIAN_POINT('',(0.0577350269189626,-0.2,0.1));
#15623=CARTESIAN_POINT('Origin',(0.,-0.2,0.));
#15624=CARTESIAN_POINT('Origin',(0.17,0.,0.));
#15625=CARTESIAN_POINT('',(-0.17,-8.67361737988404E-18,-2.0818995585505E-17));
#15626=CARTESIAN_POINT('Origin',(0.,0.,0.));
#15627=CARTESIAN_POINT('Origin',(0.,-0.015,0.));
#15628=CARTESIAN_POINT('',(-0.1954,-0.0254,-2.39295984553393E-17));
#15629=CARTESIAN_POINT('Origin',(0.,-0.0254,0.));
#15630=CARTESIAN_POINT('',(-0.185,-0.015,-2.2655965784226E-17));
#15631=CARTESIAN_POINT('Origin',(0.,-0.2775,0.));
#15632=CARTESIAN_POINT('',(-0.1954,-0.2775,-2.39295984553393E-17));
#15633=CARTESIAN_POINT('',(0.,0.,0.));
#15634=CARTESIAN_POINT('',(0.,0.,0.));
#15635=CARTESIAN_POINT('Origin',(0.,2.,8.7));
#15636=CARTESIAN_POINT('',(-0.5,2.,8.8));
#15637=CARTESIAN_POINT('Origin',(0.,2.,8.8));
#15638=CARTESIAN_POINT('',(-0.5,2.,9.6));
#15639=CARTESIAN_POINT('',(-0.5,2.,8.7));
#15640=CARTESIAN_POINT('Origin',(0.,2.,9.6));
#15641=CARTESIAN_POINT('Origin',(10.,2.,8.7));
#15642=CARTESIAN_POINT('',(9.5,2.,8.8));
#15643=CARTESIAN_POINT('Origin',(10.,2.,8.8));
#15644=CARTESIAN_POINT('',(9.5,2.,9.6));
#15645=CARTESIAN_POINT('',(9.5,2.,8.7));
#15646=CARTESIAN_POINT('Origin',(10.,2.,9.6));
#15647=CARTESIAN_POINT('Origin',(10.,2.,8.8));
#15648=CARTESIAN_POINT('',(9.37550020016016,2.5,9.6));
#15649=CARTESIAN_POINT('',(9.37550020016016,2.5,8.8));
#15650=CARTESIAN_POINT('',(9.37550020016016,2.5,8.8));
#15651=CARTESIAN_POINT('',(9.37550020016016,1.5,9.6));
#15652=CARTESIAN_POINT('Origin',(10.,2.,9.6));
#15653=CARTESIAN_POINT('',(9.37550020016016,1.5,8.8));
#15654=CARTESIAN_POINT('',(9.37550020016016,1.5,8.8));
#15655=CARTESIAN_POINT('Origin',(10.,2.,8.8));
#15656=CARTESIAN_POINT('Origin',(10.,2.5,8.8));
#15657=CARTESIAN_POINT('',(0.62449979983984,2.5,8.8));
#15658=CARTESIAN_POINT('',(0.,2.5,8.8));
#15659=CARTESIAN_POINT('',(0.62449979983984,2.5,9.6));
#15660=CARTESIAN_POINT('',(0.62449979983984,2.5,8.8));
#15661=CARTESIAN_POINT('',(0.,2.5,9.6));
#15662=CARTESIAN_POINT('Origin',(0.,2.,8.8));
#15663=CARTESIAN_POINT('',(0.62449979983984,1.5,8.8));
#15664=CARTESIAN_POINT('',(10.,1.5,8.8));
#15665=CARTESIAN_POINT('Origin',(0.,2.,8.8));
#15666=CARTESIAN_POINT('Origin',(0.,1.5,8.8));
#15667=CARTESIAN_POINT('',(0.62449979983984,1.5,9.6));
#15668=CARTESIAN_POINT('',(10.,1.5,9.6));
#15669=CARTESIAN_POINT('',(0.62449979983984,1.5,8.8));
#15670=CARTESIAN_POINT('Origin',(0.,2.,8.8));
#15671=CARTESIAN_POINT('Origin',(0.,2.,9.6));
#15672=CARTESIAN_POINT('Origin',(0.,2.,9.6));
#15673=CARTESIAN_POINT('',(0.,0.,0.));
#15674=CARTESIAN_POINT('Origin',(0.,2.,8.8));
#15675=CARTESIAN_POINT('',(-0.305,2.,9.6));
#15676=CARTESIAN_POINT('Origin',(0.,2.,9.6));
#15677=CARTESIAN_POINT('',(-0.305,2.,8.8));
#15678=CARTESIAN_POINT('',(-0.305,2.,8.8));
#15679=CARTESIAN_POINT('Origin',(0.,2.,8.8));
#15680=CARTESIAN_POINT('Origin',(0.,2.,8.8));
#15681=CARTESIAN_POINT('',(-0.5,2.,9.6));
#15682=CARTESIAN_POINT('Origin',(0.,2.,9.6));
#15683=CARTESIAN_POINT('',(-0.5,2.,8.8));
#15684=CARTESIAN_POINT('',(-0.5,2.,8.8));
#15685=CARTESIAN_POINT('Origin',(0.,2.,8.8));
#15686=CARTESIAN_POINT('Origin',(0.,2.,9.6));
#15687=CARTESIAN_POINT('Origin',(0.,2.,8.8));
#15688=CARTESIAN_POINT('',(0.,0.,0.));
#15689=CARTESIAN_POINT('Origin',(10.,2.,8.8));
#15690=CARTESIAN_POINT('',(9.695,2.,9.6));
#15691=CARTESIAN_POINT('Origin',(10.,2.,9.6));
#15692=CARTESIAN_POINT('',(9.695,2.,8.8));
#15693=CARTESIAN_POINT('',(9.695,2.,8.8));
#15694=CARTESIAN_POINT('Origin',(10.,2.,8.8));
#15695=CARTESIAN_POINT('Origin',(10.,2.,8.8));
#15696=CARTESIAN_POINT('',(9.5,2.,9.6));
#15697=CARTESIAN_POINT('Origin',(10.,2.,9.6));
#15698=CARTESIAN_POINT('',(9.5,2.,8.8));
#15699=CARTESIAN_POINT('',(9.5,2.,8.8));
#15700=CARTESIAN_POINT('Origin',(10.,2.,8.8));
#15701=CARTESIAN_POINT('Origin',(10.,2.,9.6));
#15702=CARTESIAN_POINT('Origin',(10.,2.,8.8));
#15703=CARTESIAN_POINT('',(0.,0.,0.));
#15704=CARTESIAN_POINT('',(0.,0.,0.));
#15705=CARTESIAN_POINT('',(0.,0.,0.));
#15706=CARTESIAN_POINT('',(0.,0.,0.));
#15707=CARTESIAN_POINT('',(0.,0.,0.));
#15708=CARTESIAN_POINT('Origin',(4.,0.,6.7));
#15709=CARTESIAN_POINT('',(3.5,-6.12323399573677E-17,6.8));
#15710=CARTESIAN_POINT('Origin',(4.,0.,6.8));
#15711=CARTESIAN_POINT('',(3.5,6.12323399573677E-17,7.6));
#15712=CARTESIAN_POINT('',(3.5,-6.12323399573677E-17,6.7));
#15713=CARTESIAN_POINT('Origin',(4.,0.,7.6));
#15714=CARTESIAN_POINT('Origin',(4.,12.,6.7));
#15715=CARTESIAN_POINT('',(3.5,12.,6.8));
#15716=CARTESIAN_POINT('Origin',(4.,12.,6.8));
#15717=CARTESIAN_POINT('',(3.5,12.,7.6));
#15718=CARTESIAN_POINT('',(3.5,12.,6.7));
#15719=CARTESIAN_POINT('Origin',(4.,12.,7.6));
#15720=CARTESIAN_POINT('Origin',(4.,12.,6.8));
#15721=CARTESIAN_POINT('',(3.5,11.3755002001602,7.6));
#15722=CARTESIAN_POINT('',(3.5,11.3755002001602,6.8));
#15723=CARTESIAN_POINT('',(3.5,11.3755002001602,6.8));
#15724=CARTESIAN_POINT('',(4.5,11.3755002001602,7.6));
#15725=CARTESIAN_POINT('Origin',(4.,12.,7.6));
#15726=CARTESIAN_POINT('',(4.5,11.3755002001602,6.8));
#15727=CARTESIAN_POINT('',(4.5,11.3755002001602,6.8));
#15728=CARTESIAN_POINT('Origin',(4.,12.,6.8));
#15729=CARTESIAN_POINT('Origin',(3.5,12.,6.8));
#15730=CARTESIAN_POINT('',(3.5,0.62449979983984,6.8));
#15731=CARTESIAN_POINT('',(3.5,0.,6.8));
#15732=CARTESIAN_POINT('',(3.5,0.62449979983984,7.6));
#15733=CARTESIAN_POINT('',(3.5,0.62449979983984,6.8));
#15734=CARTESIAN_POINT('',(3.5,0.,7.6));
#15735=CARTESIAN_POINT('Origin',(4.,0.,6.8));
#15736=CARTESIAN_POINT('',(4.5,0.62449979983984,6.8));
#15737=CARTESIAN_POINT('',(4.5,12.,6.8));
#15738=CARTESIAN_POINT('Origin',(4.,0.,6.8));
#15739=CARTESIAN_POINT('Origin',(4.5,0.,6.8));
#15740=CARTESIAN_POINT('',(4.5,0.62449979983984,7.6));
#15741=CARTESIAN_POINT('',(4.5,12.,7.6));
#15742=CARTESIAN_POINT('',(4.5,0.62449979983984,6.8));
#15743=CARTESIAN_POINT('Origin',(4.,0.,6.8));
#15744=CARTESIAN_POINT('Origin',(4.,0.,7.6));
#15745=CARTESIAN_POINT('Origin',(4.,0.,7.6));
#15746=CARTESIAN_POINT('',(0.,0.,0.));
#15747=CARTESIAN_POINT('Origin',(4.,0.,6.8));
#15748=CARTESIAN_POINT('',(3.695,-3.73517273739942E-17,7.6));
#15749=CARTESIAN_POINT('Origin',(4.,0.,7.6));
#15750=CARTESIAN_POINT('',(3.695,-3.73517273739942E-17,6.8));
#15751=CARTESIAN_POINT('',(3.695,-3.73517273739942E-17,6.8));
#15752=CARTESIAN_POINT('Origin',(4.,0.,6.8));
#15753=CARTESIAN_POINT('Origin',(4.,0.,6.8));
#15754=CARTESIAN_POINT('',(3.5,-6.12323399573677E-17,7.6));
#15755=CARTESIAN_POINT('Origin',(4.,0.,7.6));
#15756=CARTESIAN_POINT('',(3.5,-6.12323399573677E-17,6.8));
#15757=CARTESIAN_POINT('',(3.5,-6.12323399573677E-17,6.8));
#15758=CARTESIAN_POINT('Origin',(4.,0.,6.8));
#15759=CARTESIAN_POINT('Origin',(4.,0.,7.6));
#15760=CARTESIAN_POINT('Origin',(4.,0.,6.8));
#15761=CARTESIAN_POINT('',(0.,0.,0.));
#15762=CARTESIAN_POINT('Origin',(4.,12.,6.8));
#15763=CARTESIAN_POINT('',(3.695,12.,7.6));
#15764=CARTESIAN_POINT('Origin',(4.,12.,7.6));
#15765=CARTESIAN_POINT('',(3.695,12.,6.8));
#15766=CARTESIAN_POINT('',(3.695,12.,6.8));
#15767=CARTESIAN_POINT('Origin',(4.,12.,6.8));
#15768=CARTESIAN_POINT('Origin',(4.,12.,6.8));
#15769=CARTESIAN_POINT('',(3.5,12.,7.6));
#15770=CARTESIAN_POINT('Origin',(4.,12.,7.6));
#15771=CARTESIAN_POINT('',(3.5,12.,6.8));
#15772=CARTESIAN_POINT('',(3.5,12.,6.8));
#15773=CARTESIAN_POINT('Origin',(4.,12.,6.8));
#15774=CARTESIAN_POINT('Origin',(4.,12.,7.6));
#15775=CARTESIAN_POINT('Origin',(4.,12.,6.8));
#15776=CARTESIAN_POINT('',(0.,0.,0.));
#15777=CARTESIAN_POINT('',(0.,0.,0.));
#15778=CARTESIAN_POINT('',(0.,0.,0.));
#15779=CARTESIAN_POINT('',(0.,0.,0.));
#15780=CARTESIAN_POINT('',(0.,0.,0.));
#15781=CARTESIAN_POINT('Origin',(10.,2.,5.19));
#15782=CARTESIAN_POINT('',(9.75,2.,5.19));
#15783=CARTESIAN_POINT('Origin',(10.,2.,5.19));
#15784=CARTESIAN_POINT('',(9.75,2.,5.7));
#15785=CARTESIAN_POINT('',(9.75,2.,5.19));
#15786=CARTESIAN_POINT('Origin',(10.,2.,5.7));
#15787=CARTESIAN_POINT('Origin',(10.,2.,5.19));
#15788=CARTESIAN_POINT('Origin',(8.4,3.2,2.8));
#15789=CARTESIAN_POINT('',(8.5,3.2,2.965));
#15790=CARTESIAN_POINT('Origin',(8.5,3.2,2.8));
#15791=CARTESIAN_POINT('',(11.5,3.2,2.965));
#15792=CARTESIAN_POINT('',(8.4,3.2,2.965));
#15793=CARTESIAN_POINT('Origin',(11.5,3.2,2.8));
#15794=CARTESIAN_POINT('Origin',(8.4,0.8,5.2));
#15795=CARTESIAN_POINT('',(8.5,0.8,5.365));
#15796=CARTESIAN_POINT('Origin',(8.5,0.8,5.2));
#15797=CARTESIAN_POINT('',(11.5,0.8,5.365));
#15798=CARTESIAN_POINT('',(8.4,0.8,5.365));
#15799=CARTESIAN_POINT('Origin',(11.5,0.8,5.2));
#15800=CARTESIAN_POINT('Origin',(8.4,0.8,2.8));
#15801=CARTESIAN_POINT('',(8.5,0.8,2.965));
#15802=CARTESIAN_POINT('Origin',(8.5,0.8,2.8));
#15803=CARTESIAN_POINT('',(11.5,0.8,2.965));
#15804=CARTESIAN_POINT('',(8.4,0.8,2.965));
#15805=CARTESIAN_POINT('Origin',(11.5,0.8,2.8));
#15806=CARTESIAN_POINT('Origin',(8.4,3.2,5.2));
#15807=CARTESIAN_POINT('',(8.5,3.2,5.365));
#15808=CARTESIAN_POINT('Origin',(8.5,3.2,5.2));
#15809=CARTESIAN_POINT('',(11.5,3.2,5.365));
#15810=CARTESIAN_POINT('',(8.4,3.2,5.365));
#15811=CARTESIAN_POINT('Origin',(11.5,3.2,5.2));
#15812=CARTESIAN_POINT('Origin',(8.4,2.,4.));
#15813=CARTESIAN_POINT('',(8.5,2.,5.05));
#15814=CARTESIAN_POINT('Origin',(8.5,2.,4.));
#15815=CARTESIAN_POINT('',(11.5,2.,5.05));
#15816=CARTESIAN_POINT('',(8.4,2.,5.05));
#15817=CARTESIAN_POINT('Origin',(11.5,2.,4.));
#15818=CARTESIAN_POINT('Origin',(11.5,3.7,2.3));
#15819=CARTESIAN_POINT('',(11.5,3.7,2.3));
#15820=CARTESIAN_POINT('',(8.5,3.7,2.3));
#15821=CARTESIAN_POINT('',(11.5,3.7,2.3));
#15822=CARTESIAN_POINT('',(8.5,3.7,5.7));
#15823=CARTESIAN_POINT('',(8.5,3.7,2.3));
#15824=CARTESIAN_POINT('',(11.5,3.7,5.7));
#15825=CARTESIAN_POINT('',(11.5,3.7,5.7));
#15826=CARTESIAN_POINT('',(11.5,3.7,2.3));
#15827=CARTESIAN_POINT('Origin',(11.5,0.3,2.3));
#15828=CARTESIAN_POINT('',(11.5,0.3,2.3));
#15829=CARTESIAN_POINT('',(11.5,0.3,2.3));
#15830=CARTESIAN_POINT('',(11.5,0.3,5.7));
#15831=CARTESIAN_POINT('',(11.5,0.3,5.7));
#15832=CARTESIAN_POINT('',(11.5,0.3,2.3));
#15833=CARTESIAN_POINT('Origin',(8.5,0.3,2.3));
#15834=CARTESIAN_POINT('',(8.5,0.3,2.3));
#15835=CARTESIAN_POINT('',(8.5,0.3,2.3));
#15836=CARTESIAN_POINT('',(8.5,0.3,5.7));
#15837=CARTESIAN_POINT('',(8.5,0.3,5.7));
#15838=CARTESIAN_POINT('',(8.5,0.3,2.3));
#15839=CARTESIAN_POINT('Origin',(8.5,3.7,2.3));
#15840=CARTESIAN_POINT('',(8.5,3.7,2.3));
#15841=CARTESIAN_POINT('',(8.5,3.7,5.7));
#15842=CARTESIAN_POINT('Origin',(10.,2.,5.7));
#15843=CARTESIAN_POINT('Origin',(10.,2.,2.3));
#15844=CARTESIAN_POINT('',(0.,0.,0.));
#15845=CARTESIAN_POINT('Origin',(8.1,3.2,2.8));
#15846=CARTESIAN_POINT('',(8.2,3.2,3.025));
#15847=CARTESIAN_POINT('Origin',(8.2,3.2,2.8));
#15848=CARTESIAN_POINT('',(8.5,3.2,3.025));
#15849=CARTESIAN_POINT('',(8.1,3.2,3.025));
#15850=CARTESIAN_POINT('Origin',(8.5,3.2,2.8));
#15851=CARTESIAN_POINT('Origin',(8.1,0.8,5.2));
#15852=CARTESIAN_POINT('',(8.2,0.8,5.425));
#15853=CARTESIAN_POINT('Origin',(8.2,0.8,5.2));
#15854=CARTESIAN_POINT('',(8.5,0.8,5.425));
#15855=CARTESIAN_POINT('',(8.1,0.8,5.425));
#15856=CARTESIAN_POINT('Origin',(8.5,0.8,5.2));
#15857=CARTESIAN_POINT('Origin',(8.1,0.8,2.8));
#15858=CARTESIAN_POINT('',(8.2,0.8,3.025));
#15859=CARTESIAN_POINT('Origin',(8.2,0.8,2.8));
#15860=CARTESIAN_POINT('',(8.5,0.8,3.025));
#15861=CARTESIAN_POINT('',(8.1,0.8,3.025));
#15862=CARTESIAN_POINT('Origin',(8.5,0.8,2.8));
#15863=CARTESIAN_POINT('Origin',(8.1,3.2,5.2));
#15864=CARTESIAN_POINT('',(8.2,3.2,5.425));
#15865=CARTESIAN_POINT('Origin',(8.2,3.2,5.2));
#15866=CARTESIAN_POINT('',(8.5,3.2,5.425));
#15867=CARTESIAN_POINT('',(8.1,3.2,5.425));
#15868=CARTESIAN_POINT('Origin',(8.5,3.2,5.2));
#15869=CARTESIAN_POINT('Origin',(8.1,2.,4.));
#15870=CARTESIAN_POINT('',(8.2,2.,4.7));
#15871=CARTESIAN_POINT('Origin',(8.2,2.,4.));
#15872=CARTESIAN_POINT('',(8.5,2.,4.7));
#15873=CARTESIAN_POINT('',(8.1,2.,4.7));
#15874=CARTESIAN_POINT('Origin',(8.5,2.,4.));
#15875=CARTESIAN_POINT('Origin',(8.5,3.7,2.3));
#15876=CARTESIAN_POINT('',(8.5,3.7,2.3));
#15877=CARTESIAN_POINT('',(8.2,3.7,2.3));
#15878=CARTESIAN_POINT('',(8.5,3.7,2.3));
#15879=CARTESIAN_POINT('',(8.2,3.7,5.7));
#15880=CARTESIAN_POINT('',(8.2,3.7,2.3));
#15881=CARTESIAN_POINT('',(8.5,3.7,5.7));
#15882=CARTESIAN_POINT('',(8.5,3.7,5.7));
#15883=CARTESIAN_POINT('',(8.5,3.7,2.3));
#15884=CARTESIAN_POINT('Origin',(8.5,0.3,2.3));
#15885=CARTESIAN_POINT('',(8.5,0.3,2.3));
#15886=CARTESIAN_POINT('',(8.5,0.3,2.3));
#15887=CARTESIAN_POINT('',(8.5,0.3,5.7));
#15888=CARTESIAN_POINT('',(8.5,0.3,5.7));
#15889=CARTESIAN_POINT('',(8.5,0.3,2.3));
#15890=CARTESIAN_POINT('Origin',(8.2,0.3,2.3));
#15891=CARTESIAN_POINT('',(8.2,0.3,2.3));
#15892=CARTESIAN_POINT('',(8.2,0.3,2.3));
#15893=CARTESIAN_POINT('',(8.2,0.3,5.7));
#15894=CARTESIAN_POINT('',(8.2,0.3,5.7));
#15895=CARTESIAN_POINT('',(8.2,0.3,2.3));
#15896=CARTESIAN_POINT('Origin',(8.2,3.7,2.3));
#15897=CARTESIAN_POINT('',(8.2,3.7,2.3));
#15898=CARTESIAN_POINT('',(8.2,3.7,5.7));
#15899=CARTESIAN_POINT('Origin',(8.35,2.,5.7));
#15900=CARTESIAN_POINT('Origin',(8.35,2.,2.3));
#15901=CARTESIAN_POINT('',(0.,0.,0.));
#15902=CARTESIAN_POINT('Origin',(11.4,3.2,2.8));
#15903=CARTESIAN_POINT('',(11.5,3.2,3.025));
#15904=CARTESIAN_POINT('Origin',(11.5,3.2,2.8));
#15905=CARTESIAN_POINT('',(11.8,3.2,3.025));
#15906=CARTESIAN_POINT('',(11.4,3.2,3.025));
#15907=CARTESIAN_POINT('Origin',(11.8,3.2,2.8));
#15908=CARTESIAN_POINT('Origin',(11.4,0.8,5.2));
#15909=CARTESIAN_POINT('',(11.5,0.8,5.425));
#15910=CARTESIAN_POINT('Origin',(11.5,0.8,5.2));
#15911=CARTESIAN_POINT('',(11.8,0.8,5.425));
#15912=CARTESIAN_POINT('',(11.4,0.8,5.425));
#15913=CARTESIAN_POINT('Origin',(11.8,0.8,5.2));
#15914=CARTESIAN_POINT('Origin',(11.4,0.8,2.8));
#15915=CARTESIAN_POINT('',(11.5,0.8,3.025));
#15916=CARTESIAN_POINT('Origin',(11.5,0.8,2.8));
#15917=CARTESIAN_POINT('',(11.8,0.8,3.025));
#15918=CARTESIAN_POINT('',(11.4,0.8,3.025));
#15919=CARTESIAN_POINT('Origin',(11.8,0.8,2.8));
#15920=CARTESIAN_POINT('Origin',(11.4,3.2,5.2));
#15921=CARTESIAN_POINT('',(11.5,3.2,5.425));
#15922=CARTESIAN_POINT('Origin',(11.5,3.2,5.2));
#15923=CARTESIAN_POINT('',(11.8,3.2,5.425));
#15924=CARTESIAN_POINT('',(11.4,3.2,5.425));
#15925=CARTESIAN_POINT('Origin',(11.8,3.2,5.2));
#15926=CARTESIAN_POINT('Origin',(11.4,2.,4.));
#15927=CARTESIAN_POINT('',(11.5,2.,4.7));
#15928=CARTESIAN_POINT('Origin',(11.5,2.,4.));
#15929=CARTESIAN_POINT('',(11.8,2.,4.7));
#15930=CARTESIAN_POINT('',(11.4,2.,4.7));
#15931=CARTESIAN_POINT('Origin',(11.8,2.,4.));
#15932=CARTESIAN_POINT('Origin',(11.8,3.7,2.3));
#15933=CARTESIAN_POINT('',(11.8,3.7,2.3));
#15934=CARTESIAN_POINT('',(11.5,3.7,2.3));
#15935=CARTESIAN_POINT('',(11.8,3.7,2.3));
#15936=CARTESIAN_POINT('',(11.5,3.7,5.7));
#15937=CARTESIAN_POINT('',(11.5,3.7,2.3));
#15938=CARTESIAN_POINT('',(11.8,3.7,5.7));
#15939=CARTESIAN_POINT('',(11.8,3.7,5.7));
#15940=CARTESIAN_POINT('',(11.8,3.7,2.3));
#15941=CARTESIAN_POINT('Origin',(11.8,0.3,2.3));
#15942=CARTESIAN_POINT('',(11.8,0.3,2.3));
#15943=CARTESIAN_POINT('',(11.8,0.3,2.3));
#15944=CARTESIAN_POINT('',(11.8,0.3,5.7));
#15945=CARTESIAN_POINT('',(11.8,0.3,5.7));
#15946=CARTESIAN_POINT('',(11.8,0.3,2.3));
#15947=CARTESIAN_POINT('Origin',(11.5,0.3,2.3));
#15948=CARTESIAN_POINT('',(11.5,0.3,2.3));
#15949=CARTESIAN_POINT('',(11.5,0.3,2.3));
#15950=CARTESIAN_POINT('',(11.5,0.3,5.7));
#15951=CARTESIAN_POINT('',(11.5,0.3,5.7));
#15952=CARTESIAN_POINT('',(11.5,0.3,2.3));
#15953=CARTESIAN_POINT('Origin',(11.5,3.7,2.3));
#15954=CARTESIAN_POINT('',(11.5,3.7,2.3));
#15955=CARTESIAN_POINT('',(11.5,3.7,5.7));
#15956=CARTESIAN_POINT('Origin',(11.65,2.,5.7));
#15957=CARTESIAN_POINT('Origin',(11.65,2.,2.3));
#15958=CARTESIAN_POINT('',(0.,0.,0.));
#15959=CARTESIAN_POINT('Origin',(10.,2.,9.1));
#15960=CARTESIAN_POINT('',(9.835,2.,9.1));
#15961=CARTESIAN_POINT('Origin',(10.,2.,9.1));
#15962=CARTESIAN_POINT('',(9.835,2.,10.1));
#15963=CARTESIAN_POINT('',(9.835,2.,9.1));
#15964=CARTESIAN_POINT('Origin',(10.,2.,10.1));
#15965=CARTESIAN_POINT('Origin',(10.,2.,9.1));
#15966=CARTESIAN_POINT('Origin',(10.,2.,6.1));
#15967=CARTESIAN_POINT('',(9.3,2.,6.1));
#15968=CARTESIAN_POINT('Origin',(10.,2.,6.1));
#15969=CARTESIAN_POINT('',(9.7,2.,6.1));
#15970=CARTESIAN_POINT('Origin',(10.,2.,6.1));
#15971=CARTESIAN_POINT('Origin',(10.,2.,5.7));
#15972=CARTESIAN_POINT('',(9.3,2.,5.7));
#15973=CARTESIAN_POINT('Origin',(10.,2.,5.7));
#15974=CARTESIAN_POINT('',(9.7,2.,5.7));
#15975=CARTESIAN_POINT('Origin',(10.,2.,5.7));
#15976=CARTESIAN_POINT('Origin',(10.,2.,5.7));
#15977=CARTESIAN_POINT('',(9.3,2.,5.7));
#15978=CARTESIAN_POINT('Origin',(10.,2.,5.2));
#15979=CARTESIAN_POINT('',(9.7,2.,5.2));
#15980=CARTESIAN_POINT('',(9.7,2.,5.2));
#15981=CARTESIAN_POINT('Origin',(10.,2.,5.2));
#15982=CARTESIAN_POINT('Origin',(10.,2.,5.2));
#15983=CARTESIAN_POINT('',(9.7,2.,10.1));
#15984=CARTESIAN_POINT('Origin',(10.,2.,10.1));
#15985=CARTESIAN_POINT('',(9.7,2.,5.2));
#15986=CARTESIAN_POINT('Origin',(10.,2.,10.1));
#15987=CARTESIAN_POINT('Origin',(10.,2.,5.2));
#15988=CARTESIAN_POINT('',(0.,0.,0.));
#15989=CARTESIAN_POINT('Origin',(10.,2.,6.1));
#15990=CARTESIAN_POINT('',(9.695,2.,8.8));
#15991=CARTESIAN_POINT('Origin',(10.,2.,8.8));
#15992=CARTESIAN_POINT('',(9.695,2.,6.1));
#15993=CARTESIAN_POINT('',(9.695,2.,6.1));
#15994=CARTESIAN_POINT('Origin',(10.,2.,6.1));
#15995=CARTESIAN_POINT('Origin',(10.,2.,6.1));
#15996=CARTESIAN_POINT('',(9.5,2.,8.8));
#15997=CARTESIAN_POINT('Origin',(10.,2.,8.8));
#15998=CARTESIAN_POINT('',(9.5,2.,6.1));
#15999=CARTESIAN_POINT('',(9.5,2.,6.1));
#16000=CARTESIAN_POINT('Origin',(10.,2.,6.1));
#16001=CARTESIAN_POINT('Origin',(10.,2.,8.8));
#16002=CARTESIAN_POINT('Origin',(10.,2.,6.1));
#16003=CARTESIAN_POINT('',(0.,0.,0.));
#16004=CARTESIAN_POINT('Origin',(10.,2.,9.6));
#16005=CARTESIAN_POINT('',(9.695,2.,10.1));
#16006=CARTESIAN_POINT('Origin',(10.,2.,10.1));
#16007=CARTESIAN_POINT('',(9.695,2.,9.6));
#16008=CARTESIAN_POINT('',(9.695,2.,9.6));
#16009=CARTESIAN_POINT('Origin',(10.,2.,9.6));
#16010=CARTESIAN_POINT('Origin',(10.,2.,9.6));
#16011=CARTESIAN_POINT('',(9.5,2.,10.1));
#16012=CARTESIAN_POINT('Origin',(10.,2.,10.1));
#16013=CARTESIAN_POINT('',(9.5,2.,9.6));
#16014=CARTESIAN_POINT('',(9.5,2.,9.6));
#16015=CARTESIAN_POINT('Origin',(10.,2.,9.6));
#16016=CARTESIAN_POINT('Origin',(10.,2.,10.1));
#16017=CARTESIAN_POINT('Origin',(10.,2.,9.6));
#16018=CARTESIAN_POINT('',(0.,0.,0.));
#16019=CARTESIAN_POINT('Origin',(10.,2.,10.1));
#16020=CARTESIAN_POINT('',(9.775,2.,10.3));
#16021=CARTESIAN_POINT('Origin',(10.,2.,10.3));
#16022=CARTESIAN_POINT('',(9.775,2.,10.1));
#16023=CARTESIAN_POINT('',(9.775,2.,10.1));
#16024=CARTESIAN_POINT('Origin',(10.,2.,10.1));
#16025=CARTESIAN_POINT('Origin',(10.,2.,10.1));
#16026=CARTESIAN_POINT('',(9.5,2.,10.3));
#16027=CARTESIAN_POINT('Origin',(10.,2.,10.3));
#16028=CARTESIAN_POINT('',(9.5,2.,10.1));
#16029=CARTESIAN_POINT('',(9.5,2.,10.1));
#16030=CARTESIAN_POINT('Origin',(10.,2.,10.1));
#16031=CARTESIAN_POINT('Origin',(10.,2.,10.3));
#16032=CARTESIAN_POINT('Origin',(10.,2.,10.1));
#16033=CARTESIAN_POINT('',(0.,0.,0.));
#16034=CARTESIAN_POINT('',(0.,0.,0.));
#16035=CARTESIAN_POINT('Origin',(4.,12.,5.19));
#16036=CARTESIAN_POINT('',(3.75,12.,5.19));
#16037=CARTESIAN_POINT('Origin',(4.,12.,5.19));
#16038=CARTESIAN_POINT('',(3.75,12.,5.7));
#16039=CARTESIAN_POINT('',(3.75,12.,5.19));
#16040=CARTESIAN_POINT('Origin',(4.,12.,5.7));
#16041=CARTESIAN_POINT('Origin',(4.,12.,5.19));
#16042=CARTESIAN_POINT('Origin',(5.2,10.4,2.8));
#16043=CARTESIAN_POINT('',(5.035,10.5,2.8));
#16044=CARTESIAN_POINT('Origin',(5.2,10.5,2.8));
#16045=CARTESIAN_POINT('',(5.035,13.5,2.8));
#16046=CARTESIAN_POINT('',(5.035,10.4,2.8));
#16047=CARTESIAN_POINT('Origin',(5.2,13.5,2.8));
#16048=CARTESIAN_POINT('Origin',(2.8,10.4,5.2));
#16049=CARTESIAN_POINT('',(2.635,10.5,5.2));
#16050=CARTESIAN_POINT('Origin',(2.8,10.5,5.2));
#16051=CARTESIAN_POINT('',(2.635,13.5,5.2));
#16052=CARTESIAN_POINT('',(2.635,10.4,5.2));
#16053=CARTESIAN_POINT('Origin',(2.8,13.5,5.2));
#16054=CARTESIAN_POINT('Origin',(2.8,10.4,2.8));
#16055=CARTESIAN_POINT('',(2.635,10.5,2.8));
#16056=CARTESIAN_POINT('Origin',(2.8,10.5,2.8));
#16057=CARTESIAN_POINT('',(2.635,13.5,2.8));
#16058=CARTESIAN_POINT('',(2.635,10.4,2.8));
#16059=CARTESIAN_POINT('Origin',(2.8,13.5,2.8));
#16060=CARTESIAN_POINT('Origin',(5.2,10.4,5.2));
#16061=CARTESIAN_POINT('',(5.035,10.5,5.2));
#16062=CARTESIAN_POINT('Origin',(5.2,10.5,5.2));
#16063=CARTESIAN_POINT('',(5.035,13.5,5.2));
#16064=CARTESIAN_POINT('',(5.035,10.4,5.2));
#16065=CARTESIAN_POINT('Origin',(5.2,13.5,5.2));
#16066=CARTESIAN_POINT('Origin',(4.,10.4,4.));
#16067=CARTESIAN_POINT('',(2.95,10.5,4.));
#16068=CARTESIAN_POINT('Origin',(4.,10.5,4.));
#16069=CARTESIAN_POINT('',(2.95,13.5,4.));
#16070=CARTESIAN_POINT('',(2.95,10.4,4.));
#16071=CARTESIAN_POINT('Origin',(4.,13.5,4.));
#16072=CARTESIAN_POINT('Origin',(5.7,13.5,2.3));
#16073=CARTESIAN_POINT('',(5.7,13.5,2.3));
#16074=CARTESIAN_POINT('',(2.3,13.5,2.3));
#16075=CARTESIAN_POINT('',(5.7,13.5,2.3));
#16076=CARTESIAN_POINT('',(2.3,13.5,5.7));
#16077=CARTESIAN_POINT('',(2.3,13.5,2.3));
#16078=CARTESIAN_POINT('',(5.7,13.5,5.7));
#16079=CARTESIAN_POINT('',(5.7,13.5,5.7));
#16080=CARTESIAN_POINT('',(5.7,13.5,2.3));
#16081=CARTESIAN_POINT('Origin',(5.7,10.5,2.3));
#16082=CARTESIAN_POINT('',(5.7,10.5,2.3));
#16083=CARTESIAN_POINT('',(5.7,10.5,2.3));
#16084=CARTESIAN_POINT('',(5.7,10.5,5.7));
#16085=CARTESIAN_POINT('',(5.7,10.5,5.7));
#16086=CARTESIAN_POINT('',(5.7,10.5,2.3));
#16087=CARTESIAN_POINT('Origin',(2.3,10.5,2.3));
#16088=CARTESIAN_POINT('',(2.3,10.5,2.3));
#16089=CARTESIAN_POINT('',(2.3,10.5,2.3));
#16090=CARTESIAN_POINT('',(2.3,10.5,5.7));
#16091=CARTESIAN_POINT('',(2.3,10.5,5.7));
#16092=CARTESIAN_POINT('',(2.3,10.5,2.3));
#16093=CARTESIAN_POINT('Origin',(2.3,13.5,2.3));
#16094=CARTESIAN_POINT('',(2.3,13.5,2.3));
#16095=CARTESIAN_POINT('',(2.3,13.5,5.7));
#16096=CARTESIAN_POINT('Origin',(4.,12.,5.7));
#16097=CARTESIAN_POINT('Origin',(4.,12.,2.3));
#16098=CARTESIAN_POINT('',(0.,0.,0.));
#16099=CARTESIAN_POINT('Origin',(5.2,10.1,2.8));
#16100=CARTESIAN_POINT('',(4.975,10.2,2.8));
#16101=CARTESIAN_POINT('Origin',(5.2,10.2,2.8));
#16102=CARTESIAN_POINT('',(4.975,10.5,2.8));
#16103=CARTESIAN_POINT('',(4.975,10.1,2.8));
#16104=CARTESIAN_POINT('Origin',(5.2,10.5,2.8));
#16105=CARTESIAN_POINT('Origin',(2.8,10.1,5.2));
#16106=CARTESIAN_POINT('',(2.575,10.2,5.2));
#16107=CARTESIAN_POINT('Origin',(2.8,10.2,5.2));
#16108=CARTESIAN_POINT('',(2.575,10.5,5.2));
#16109=CARTESIAN_POINT('',(2.575,10.1,5.2));
#16110=CARTESIAN_POINT('Origin',(2.8,10.5,5.2));
#16111=CARTESIAN_POINT('Origin',(2.8,10.1,2.8));
#16112=CARTESIAN_POINT('',(2.575,10.2,2.8));
#16113=CARTESIAN_POINT('Origin',(2.8,10.2,2.8));
#16114=CARTESIAN_POINT('',(2.575,10.5,2.8));
#16115=CARTESIAN_POINT('',(2.575,10.1,2.8));
#16116=CARTESIAN_POINT('Origin',(2.8,10.5,2.8));
#16117=CARTESIAN_POINT('Origin',(5.2,10.1,5.2));
#16118=CARTESIAN_POINT('',(4.975,10.2,5.2));
#16119=CARTESIAN_POINT('Origin',(5.2,10.2,5.2));
#16120=CARTESIAN_POINT('',(4.975,10.5,5.2));
#16121=CARTESIAN_POINT('',(4.975,10.1,5.2));
#16122=CARTESIAN_POINT('Origin',(5.2,10.5,5.2));
#16123=CARTESIAN_POINT('Origin',(4.,10.1,4.));
#16124=CARTESIAN_POINT('',(3.3,10.2,4.));
#16125=CARTESIAN_POINT('Origin',(4.,10.2,4.));
#16126=CARTESIAN_POINT('',(3.3,10.5,4.));
#16127=CARTESIAN_POINT('',(3.3,10.1,4.));
#16128=CARTESIAN_POINT('Origin',(4.,10.5,4.));
#16129=CARTESIAN_POINT('Origin',(5.7,10.5,2.3));
#16130=CARTESIAN_POINT('',(5.7,10.5,2.3));
#16131=CARTESIAN_POINT('',(2.3,10.5,2.3));
#16132=CARTESIAN_POINT('',(5.7,10.5,2.3));
#16133=CARTESIAN_POINT('',(2.3,10.5,5.7));
#16134=CARTESIAN_POINT('',(2.3,10.5,2.3));
#16135=CARTESIAN_POINT('',(5.7,10.5,5.7));
#16136=CARTESIAN_POINT('',(5.7,10.5,5.7));
#16137=CARTESIAN_POINT('',(5.7,10.5,2.3));
#16138=CARTESIAN_POINT('Origin',(5.7,10.2,2.3));
#16139=CARTESIAN_POINT('',(5.7,10.2,2.3));
#16140=CARTESIAN_POINT('',(5.7,10.2,2.3));
#16141=CARTESIAN_POINT('',(5.7,10.2,5.7));
#16142=CARTESIAN_POINT('',(5.7,10.2,5.7));
#16143=CARTESIAN_POINT('',(5.7,10.2,2.3));
#16144=CARTESIAN_POINT('Origin',(2.3,10.2,2.3));
#16145=CARTESIAN_POINT('',(2.3,10.2,2.3));
#16146=CARTESIAN_POINT('',(2.3,10.2,2.3));
#16147=CARTESIAN_POINT('',(2.3,10.2,5.7));
#16148=CARTESIAN_POINT('',(2.3,10.2,5.7));
#16149=CARTESIAN_POINT('',(2.3,10.2,2.3));
#16150=CARTESIAN_POINT('Origin',(2.3,10.5,2.3));
#16151=CARTESIAN_POINT('',(2.3,10.5,2.3));
#16152=CARTESIAN_POINT('',(2.3,10.5,5.7));
#16153=CARTESIAN_POINT('Origin',(4.,10.35,5.7));
#16154=CARTESIAN_POINT('Origin',(4.,10.35,2.3));
#16155=CARTESIAN_POINT('',(0.,0.,0.));
#16156=CARTESIAN_POINT('Origin',(5.2,13.4,2.8));
#16157=CARTESIAN_POINT('',(4.975,13.5,2.8));
#16158=CARTESIAN_POINT('Origin',(5.2,13.5,2.8));
#16159=CARTESIAN_POINT('',(4.975,13.8,2.8));
#16160=CARTESIAN_POINT('',(4.975,13.4,2.8));
#16161=CARTESIAN_POINT('Origin',(5.2,13.8,2.8));
#16162=CARTESIAN_POINT('Origin',(2.8,13.4,5.2));
#16163=CARTESIAN_POINT('',(2.575,13.5,5.2));
#16164=CARTESIAN_POINT('Origin',(2.8,13.5,5.2));
#16165=CARTESIAN_POINT('',(2.575,13.8,5.2));
#16166=CARTESIAN_POINT('',(2.575,13.4,5.2));
#16167=CARTESIAN_POINT('Origin',(2.8,13.8,5.2));
#16168=CARTESIAN_POINT('Origin',(2.8,13.4,2.8));
#16169=CARTESIAN_POINT('',(2.575,13.5,2.8));
#16170=CARTESIAN_POINT('Origin',(2.8,13.5,2.8));
#16171=CARTESIAN_POINT('',(2.575,13.8,2.8));
#16172=CARTESIAN_POINT('',(2.575,13.4,2.8));
#16173=CARTESIAN_POINT('Origin',(2.8,13.8,2.8));
#16174=CARTESIAN_POINT('Origin',(5.2,13.4,5.2));
#16175=CARTESIAN_POINT('',(4.975,13.5,5.2));
#16176=CARTESIAN_POINT('Origin',(5.2,13.5,5.2));
#16177=CARTESIAN_POINT('',(4.975,13.8,5.2));
#16178=CARTESIAN_POINT('',(4.975,13.4,5.2));
#16179=CARTESIAN_POINT('Origin',(5.2,13.8,5.2));
#16180=CARTESIAN_POINT('Origin',(4.,13.4,4.));
#16181=CARTESIAN_POINT('',(3.3,13.5,4.));
#16182=CARTESIAN_POINT('Origin',(4.,13.5,4.));
#16183=CARTESIAN_POINT('',(3.3,13.8,4.));
#16184=CARTESIAN_POINT('',(3.3,13.4,4.));
#16185=CARTESIAN_POINT('Origin',(4.,13.8,4.));
#16186=CARTESIAN_POINT('Origin',(5.7,13.8,2.3));
#16187=CARTESIAN_POINT('',(5.7,13.8,2.3));
#16188=CARTESIAN_POINT('',(2.3,13.8,2.3));
#16189=CARTESIAN_POINT('',(5.7,13.8,2.3));
#16190=CARTESIAN_POINT('',(2.3,13.8,5.7));
#16191=CARTESIAN_POINT('',(2.3,13.8,2.3));
#16192=CARTESIAN_POINT('',(5.7,13.8,5.7));
#16193=CARTESIAN_POINT('',(5.7,13.8,5.7));
#16194=CARTESIAN_POINT('',(5.7,13.8,2.3));
#16195=CARTESIAN_POINT('Origin',(5.7,13.5,2.3));
#16196=CARTESIAN_POINT('',(5.7,13.5,2.3));
#16197=CARTESIAN_POINT('',(5.7,13.5,2.3));
#16198=CARTESIAN_POINT('',(5.7,13.5,5.7));
#16199=CARTESIAN_POINT('',(5.7,13.5,5.7));
#16200=CARTESIAN_POINT('',(5.7,13.5,2.3));
#16201=CARTESIAN_POINT('Origin',(2.3,13.5,2.3));
#16202=CARTESIAN_POINT('',(2.3,13.5,2.3));
#16203=CARTESIAN_POINT('',(2.3,13.5,2.3));
#16204=CARTESIAN_POINT('',(2.3,13.5,5.7));
#16205=CARTESIAN_POINT('',(2.3,13.5,5.7));
#16206=CARTESIAN_POINT('',(2.3,13.5,2.3));
#16207=CARTESIAN_POINT('Origin',(2.3,13.8,2.3));
#16208=CARTESIAN_POINT('',(2.3,13.8,2.3));
#16209=CARTESIAN_POINT('',(2.3,13.8,5.7));
#16210=CARTESIAN_POINT('Origin',(4.,13.65,5.7));
#16211=CARTESIAN_POINT('Origin',(4.,13.65,2.3));
#16212=CARTESIAN_POINT('',(0.,0.,0.));
#16213=CARTESIAN_POINT('Origin',(4.,12.,7.1));
#16214=CARTESIAN_POINT('',(3.835,12.,7.1));
#16215=CARTESIAN_POINT('Origin',(4.,12.,7.1));
#16216=CARTESIAN_POINT('',(3.835,12.,8.1));
#16217=CARTESIAN_POINT('',(3.835,12.,7.1));
#16218=CARTESIAN_POINT('Origin',(4.,12.,8.1));
#16219=CARTESIAN_POINT('Origin',(4.,12.,7.1));
#16220=CARTESIAN_POINT('Origin',(4.,12.,6.1));
#16221=CARTESIAN_POINT('',(3.3,12.,6.1));
#16222=CARTESIAN_POINT('Origin',(4.,12.,6.1));
#16223=CARTESIAN_POINT('',(3.7,12.,6.1));
#16224=CARTESIAN_POINT('Origin',(4.,12.,6.1));
#16225=CARTESIAN_POINT('Origin',(4.,12.,5.7));
#16226=CARTESIAN_POINT('',(3.3,12.,5.7));
#16227=CARTESIAN_POINT('Origin',(4.,12.,5.7));
#16228=CARTESIAN_POINT('',(3.7,12.,5.7));
#16229=CARTESIAN_POINT('Origin',(4.,12.,5.7));
#16230=CARTESIAN_POINT('Origin',(4.,12.,5.7));
#16231=CARTESIAN_POINT('',(3.3,12.,5.7));
#16232=CARTESIAN_POINT('Origin',(4.,12.,5.2));
#16233=CARTESIAN_POINT('',(3.7,12.,5.2));
#16234=CARTESIAN_POINT('',(3.7,12.,5.2));
#16235=CARTESIAN_POINT('Origin',(4.,12.,5.2));
#16236=CARTESIAN_POINT('Origin',(4.,12.,5.2));
#16237=CARTESIAN_POINT('',(3.7,12.,8.1));
#16238=CARTESIAN_POINT('Origin',(4.,12.,8.1));
#16239=CARTESIAN_POINT('',(3.7,12.,5.2));
#16240=CARTESIAN_POINT('Origin',(4.,12.,8.1));
#16241=CARTESIAN_POINT('Origin',(4.,12.,5.2));
#16242=CARTESIAN_POINT('',(0.,0.,0.));
#16243=CARTESIAN_POINT('Origin',(4.,12.,6.1));
#16244=CARTESIAN_POINT('',(3.695,12.,6.8));
#16245=CARTESIAN_POINT('Origin',(4.,12.,6.8));
#16246=CARTESIAN_POINT('',(3.695,12.,6.1));
#16247=CARTESIAN_POINT('',(3.695,12.,6.1));
#16248=CARTESIAN_POINT('Origin',(4.,12.,6.1));
#16249=CARTESIAN_POINT('Origin',(4.,12.,6.1));
#16250=CARTESIAN_POINT('',(3.5,12.,6.8));
#16251=CARTESIAN_POINT('Origin',(4.,12.,6.8));
#16252=CARTESIAN_POINT('',(3.5,12.,6.1));
#16253=CARTESIAN_POINT('',(3.5,12.,6.1));
#16254=CARTESIAN_POINT('Origin',(4.,12.,6.1));
#16255=CARTESIAN_POINT('Origin',(4.,12.,6.8));
#16256=CARTESIAN_POINT('Origin',(4.,12.,6.1));
#16257=CARTESIAN_POINT('',(0.,0.,0.));
#16258=CARTESIAN_POINT('Origin',(4.,12.,7.6));
#16259=CARTESIAN_POINT('',(3.695,12.,8.1));
#16260=CARTESIAN_POINT('Origin',(4.,12.,8.1));
#16261=CARTESIAN_POINT('',(3.695,12.,7.6));
#16262=CARTESIAN_POINT('',(3.695,12.,7.6));
#16263=CARTESIAN_POINT('Origin',(4.,12.,7.6));
#16264=CARTESIAN_POINT('Origin',(4.,12.,7.6));
#16265=CARTESIAN_POINT('',(3.5,12.,8.1));
#16266=CARTESIAN_POINT('Origin',(4.,12.,8.1));
#16267=CARTESIAN_POINT('',(3.5,12.,7.6));
#16268=CARTESIAN_POINT('',(3.5,12.,7.6));
#16269=CARTESIAN_POINT('Origin',(4.,12.,7.6));
#16270=CARTESIAN_POINT('Origin',(4.,12.,8.1));
#16271=CARTESIAN_POINT('Origin',(4.,12.,7.6));
#16272=CARTESIAN_POINT('',(0.,0.,0.));
#16273=CARTESIAN_POINT('Origin',(4.,12.,8.1));
#16274=CARTESIAN_POINT('',(3.775,12.,8.3));
#16275=CARTESIAN_POINT('Origin',(4.,12.,8.3));
#16276=CARTESIAN_POINT('',(3.775,12.,8.1));
#16277=CARTESIAN_POINT('',(3.775,12.,8.1));
#16278=CARTESIAN_POINT('Origin',(4.,12.,8.1));
#16279=CARTESIAN_POINT('Origin',(4.,12.,8.1));
#16280=CARTESIAN_POINT('',(3.5,12.,8.3));
#16281=CARTESIAN_POINT('Origin',(4.,12.,8.3));
#16282=CARTESIAN_POINT('',(3.5,12.,8.1));
#16283=CARTESIAN_POINT('',(3.5,12.,8.1));
#16284=CARTESIAN_POINT('Origin',(4.,12.,8.1));
#16285=CARTESIAN_POINT('Origin',(4.,12.,8.3));
#16286=CARTESIAN_POINT('Origin',(4.,12.,8.1));
#16287=CARTESIAN_POINT('',(0.,0.,0.));
#16288=CARTESIAN_POINT('',(0.,0.,0.));
#16289=CARTESIAN_POINT('Origin',(0.75,1.2,0.));
#16290=CARTESIAN_POINT('',(0.885663593019381,1.2,-0.16));
#16291=CARTESIAN_POINT('',(0.885663593019381,1.2,0.16));
#16292=CARTESIAN_POINT('Origin',(0.,1.2,0.));
#16293=CARTESIAN_POINT('',(0.93,1.2,-0.16));
#16294=CARTESIAN_POINT('',(0.93,1.2,-0.16));
#16295=CARTESIAN_POINT('',(0.93,1.2,0.16));
#16296=CARTESIAN_POINT('',(0.93,1.2,0.16));
#16297=CARTESIAN_POINT('',(0.57,1.2,0.16));
#16298=CARTESIAN_POINT('Origin',(0.57,0.,0.16));
#16299=CARTESIAN_POINT('',(0.885663593019381,-1.2,0.16));
#16300=CARTESIAN_POINT('',(0.885663593019381,0.,0.16));
#16301=CARTESIAN_POINT('',(0.93,-1.2,0.16));
#16302=CARTESIAN_POINT('',(0.93,0.,0.16));
#16303=CARTESIAN_POINT('',(0.57,-1.2,0.16));
#16304=CARTESIAN_POINT('Origin',(0.75,-1.2,0.));
#16305=CARTESIAN_POINT('',(0.885663593019381,-1.2,-0.16));
#16306=CARTESIAN_POINT('Origin',(0.,-1.2,0.));
#16307=CARTESIAN_POINT('',(0.93,-1.2,-0.16));
#16308=CARTESIAN_POINT('',(0.93,-1.2,0.16));
#16309=CARTESIAN_POINT('',(0.93,-1.2,-0.16));
#16310=CARTESIAN_POINT('Origin',(0.93,0.,-0.16));
#16311=CARTESIAN_POINT('',(0.885663593019381,0.,-0.16));
#16312=CARTESIAN_POINT('',(0.93,0.,-0.16));
#16313=CARTESIAN_POINT('Origin',(0.93,0.,0.16));
#16314=CARTESIAN_POINT('Origin',(1.05,1.5,0.));
#16315=CARTESIAN_POINT('',(-1.05,1.5,-1.28587913910472E-16));
#16316=CARTESIAN_POINT('Origin',(0.,1.5,0.));
#16317=CARTESIAN_POINT('',(-0.9,1.5,-1.10218211923262E-16));
#16318=CARTESIAN_POINT('Origin',(0.,1.5,0.));
#16319=CARTESIAN_POINT('Origin',(0.,1.315,0.));
#16320=CARTESIAN_POINT('',(-1.05,1.13,-1.28587913910472E-16));
#16321=CARTESIAN_POINT('Origin',(0.,1.13,0.));
#16322=CARTESIAN_POINT('',(-1.05,1.315,-1.28587913910472E-16));
#16323=CARTESIAN_POINT('Origin',(1.,1.13,0.));
#16324=CARTESIAN_POINT('',(-1.,1.13,-1.22464679914735E-16));
#16325=CARTESIAN_POINT('Origin',(0.,1.13,0.));
#16326=CARTESIAN_POINT('Origin',(0.,1.065,0.));
#16327=CARTESIAN_POINT('',(-1.,1.,-1.22464679914735E-16));
#16328=CARTESIAN_POINT('Origin',(0.,1.,0.));
#16329=CARTESIAN_POINT('',(-1.,1.065,-1.22464679914735E-16));
#16330=CARTESIAN_POINT('Origin',(1.05,1.,0.));
#16331=CARTESIAN_POINT('',(-1.05,1.,-1.28587913910472E-16));
#16332=CARTESIAN_POINT('Origin',(0.,1.,0.));
#16333=CARTESIAN_POINT('Origin',(0.,0.,0.));
#16334=CARTESIAN_POINT('',(-1.05,-1.,-1.28587913910472E-16));
#16335=CARTESIAN_POINT('Origin',(0.,-1.,0.));
#16336=CARTESIAN_POINT('',(-1.05,0.,-1.28587913910472E-16));
#16337=CARTESIAN_POINT('Origin',(1.,-1.,0.));
#16338=CARTESIAN_POINT('',(-1.,-1.,-1.22464679914735E-16));
#16339=CARTESIAN_POINT('Origin',(0.,-1.,0.));
#16340=CARTESIAN_POINT('Origin',(0.,-1.065,0.));
#16341=CARTESIAN_POINT('',(-1.,-1.13,-1.22464679914735E-16));
#16342=CARTESIAN_POINT('Origin',(0.,-1.13,0.));
#16343=CARTESIAN_POINT('',(-1.,-1.065,-1.22464679914735E-16));
#16344=CARTESIAN_POINT('Origin',(1.05,-1.13,0.));
#16345=CARTESIAN_POINT('',(-1.05,-1.13,-1.28587913910472E-16));
#16346=CARTESIAN_POINT('Origin',(0.,-1.13,0.));
#16347=CARTESIAN_POINT('Origin',(0.,-1.315,0.));
#16348=CARTESIAN_POINT('',(-1.05,-1.5,-1.28587913910472E-16));
#16349=CARTESIAN_POINT('Origin',(0.,-1.5,0.));
#16350=CARTESIAN_POINT('',(-1.05,-1.315,-1.28587913910472E-16));
#16351=CARTESIAN_POINT('Origin',(0.9,-1.5,0.));
#16352=CARTESIAN_POINT('',(-0.9,-1.5,-1.10218211923262E-16));
#16353=CARTESIAN_POINT('Origin',(0.,-1.5,0.));
#16354=CARTESIAN_POINT('Origin',(0.,0.,0.));
#16355=CARTESIAN_POINT('',(-0.9,0.,-1.10218211923262E-16));
#16356=CARTESIAN_POINT('',(0.,0.,0.));
#16357=CARTESIAN_POINT('Origin',(0.75,1.2,0.));
#16358=CARTESIAN_POINT('',(0.880582193778639,1.2,0.16));
#16359=CARTESIAN_POINT('',(0.880582193778639,1.2,-0.16));
#16360=CARTESIAN_POINT('Origin',(0.,1.2,0.));
#16361=CARTESIAN_POINT('',(0.583459510163302,1.2,0.16));
#16362=CARTESIAN_POINT('',(0.57,1.2,0.16));
#16363=CARTESIAN_POINT('',(0.583459510163302,1.2,-0.16));
#16364=CARTESIAN_POINT('Origin',(0.,1.2,0.));
#16365=CARTESIAN_POINT('',(0.93,1.2,-0.16));
#16366=CARTESIAN_POINT('Origin',(0.93,0.,-0.16));
#16367=CARTESIAN_POINT('',(0.880582193778639,-1.2,-0.16));
#16368=CARTESIAN_POINT('',(0.880582193778639,0.,-0.16));
#16369=CARTESIAN_POINT('',(0.583459510163302,-1.2,-0.16));
#16370=CARTESIAN_POINT('',(0.583459510163302,0.,-0.16));
#16371=CARTESIAN_POINT('',(0.93,-1.2,-0.16));
#16372=CARTESIAN_POINT('Origin',(0.75,-1.2,0.));
#16373=CARTESIAN_POINT('',(0.880582193778639,-1.2,0.16));
#16374=CARTESIAN_POINT('Origin',(0.,-1.2,0.));
#16375=CARTESIAN_POINT('',(0.583459510163302,-1.2,0.16));
#16376=CARTESIAN_POINT('Origin',(0.,-1.2,0.));
#16377=CARTESIAN_POINT('',(0.57,-1.2,0.16));
#16378=CARTESIAN_POINT('Origin',(0.57,0.,0.16));
#16379=CARTESIAN_POINT('',(0.880582193778639,0.,0.16));
#16380=CARTESIAN_POINT('',(0.583459510163302,0.,0.16));
#16381=CARTESIAN_POINT('Origin',(0.895,1.35,0.));
#16382=CARTESIAN_POINT('',(-0.895,1.35,-1.09605888523688E-16));
#16383=CARTESIAN_POINT('Origin',(0.,1.35,0.));
#16384=CARTESIAN_POINT('',(-0.605,1.35,-7.40911313484149E-17));
#16385=CARTESIAN_POINT('Origin',(0.,1.35,0.));
#16386=CARTESIAN_POINT('Origin',(0.,0.,0.));
#16387=CARTESIAN_POINT('',(-0.895,-1.35,-1.09605888523688E-16));
#16388=CARTESIAN_POINT('Origin',(0.,-1.35,0.));
#16389=CARTESIAN_POINT('',(-0.895,0.,-1.09605888523688E-16));
#16390=CARTESIAN_POINT('Origin',(0.605,-1.35,0.));
#16391=CARTESIAN_POINT('',(-0.605,-1.35,-7.40911313484149E-17));
#16392=CARTESIAN_POINT('Origin',(0.,-1.35,0.));
#16393=CARTESIAN_POINT('Origin',(0.,0.,0.));
#16394=CARTESIAN_POINT('',(-0.605,0.,-7.40911313484149E-17));
#16395=CARTESIAN_POINT('',(0.,0.,0.));
#16396=CARTESIAN_POINT('',(0.,0.,0.));
#16397=CARTESIAN_POINT('',(0.,0.,0.));
#16398=CARTESIAN_POINT('Origin',(0.0866025403784439,-0.4,-0.15));
#16399=CARTESIAN_POINT('',(0.173205080756888,-0.4,0.));
#16400=CARTESIAN_POINT('',(0.0866025403784439,-0.4,-0.15));
#16401=CARTESIAN_POINT('',(0.173205080756888,-0.4,0.));
#16402=CARTESIAN_POINT('',(0.0866025403784439,-0.64,-0.15));
#16403=CARTESIAN_POINT('',(0.0866025403784439,-0.4,-0.15));
#16404=CARTESIAN_POINT('',(0.173205080756888,-0.64,0.));
#16405=CARTESIAN_POINT('',(0.173205080756888,-0.64,0.));
#16406=CARTESIAN_POINT('',(0.173205080756888,-0.4,0.));
#16407=CARTESIAN_POINT('Origin',(-0.0866025403784438,-0.4,-0.15));
#16408=CARTESIAN_POINT('',(-0.0866025403784438,-0.4,-0.15));
#16409=CARTESIAN_POINT('',(0.0866025403784439,-0.4,-0.15));
#16410=CARTESIAN_POINT('',(-0.0866025403784438,-0.64,-0.15));
#16411=CARTESIAN_POINT('',(-0.0866025403784438,-0.4,-0.15));
#16412=CARTESIAN_POINT('',(0.0866025403784439,-0.64,-0.15));
#16413=CARTESIAN_POINT('Origin',(-0.173205080756888,-0.4,-2.77555756156289E-17));
#16414=CARTESIAN_POINT('',(-0.173205080756888,-0.4,-2.12115047744981E-17));
#16415=CARTESIAN_POINT('',(-0.0866025403784438,-0.4,-0.15));
#16416=CARTESIAN_POINT('',(-0.173205080756888,-0.64,-2.77555756156289E-17));
#16417=CARTESIAN_POINT('',(-0.173205080756888,-0.4,-2.12115047744981E-17));
#16418=CARTESIAN_POINT('',(-0.0866025403784438,-0.64,-0.15));
#16419=CARTESIAN_POINT('Origin',(-0.0866025403784439,-0.4,0.15));
#16420=CARTESIAN_POINT('',(-0.0866025403784439,-0.4,0.15));
#16421=CARTESIAN_POINT('',(-0.173205080756888,-0.4,-2.12115047744981E-17));
#16422=CARTESIAN_POINT('',(-0.0866025403784439,-0.64,0.15));
#16423=CARTESIAN_POINT('',(-0.0866025403784439,-0.4,0.15));
#16424=CARTESIAN_POINT('',(-0.173205080756888,-0.64,-2.12115047744981E-17));
#16425=CARTESIAN_POINT('Origin',(0.0866025403784439,-0.4,0.15));
#16426=CARTESIAN_POINT('',(0.0866025403784439,-0.4,0.15));
#16427=CARTESIAN_POINT('',(-0.0866025403784439,-0.4,0.15));
#16428=CARTESIAN_POINT('',(0.0866025403784439,-0.64,0.15));
#16429=CARTESIAN_POINT('',(0.0866025403784439,-0.4,0.15));
#16430=CARTESIAN_POINT('',(-0.0866025403784439,-0.64,0.15));
#16431=CARTESIAN_POINT('Origin',(0.173205080756888,-0.4,0.));
#16432=CARTESIAN_POINT('',(0.0866025403784439,-0.4,0.15));
#16433=CARTESIAN_POINT('',(0.0866025403784439,-0.64,0.15));
#16434=CARTESIAN_POINT('Origin',(0.,-0.4,-2.77555756156289E-17));
#16435=CARTESIAN_POINT('Origin',(0.,-0.64,-2.77555756156289E-17));
#16436=CARTESIAN_POINT('Origin',(0.,-1.,0.));
#16437=CARTESIAN_POINT('',(-0.1954,-1.,2.39295984553393E-17));
#16438=CARTESIAN_POINT('Origin',(0.,-1.,0.));
#16439=CARTESIAN_POINT('Origin',(0.3,0.4,0.));
#16440=CARTESIAN_POINT('',(-0.3,0.4,-3.67394039744206E-17));
#16441=CARTESIAN_POINT('Origin',(0.,0.4,0.));
#16442=CARTESIAN_POINT('Origin',(0.,0.375,0.));
#16443=CARTESIAN_POINT('',(-0.35,0.35,-4.28626379701573E-17));
#16444=CARTESIAN_POINT('Origin',(0.,0.35,0.));
#16445=CARTESIAN_POINT('',(-0.325,0.375,-3.9801020972289E-17));
#16446=CARTESIAN_POINT('Origin',(0.,0.19,0.));
#16447=CARTESIAN_POINT('',(-0.35,0.03,-4.28626379701574E-17));
#16448=CARTESIAN_POINT('Origin',(0.,0.03,0.));
#16449=CARTESIAN_POINT('',(-0.35,0.19,-4.28626379701574E-17));
#16450=CARTESIAN_POINT('Origin',(0.,0.0149999999999999,0.));
#16451=CARTESIAN_POINT('',(-0.32,-3.29597460435593E-17,-3.91886975727153E-17));
#16452=CARTESIAN_POINT('Origin',(0.,0.,0.));
#16453=CARTESIAN_POINT('',(-0.335,0.0149999999999999,-4.10256677714363E-17));
#16454=CARTESIAN_POINT('Origin',(0.22,0.,0.));
#16455=CARTESIAN_POINT('',(-0.22,-6.93889390390723E-18,-2.69422295812418E-17));
#16456=CARTESIAN_POINT('Origin',(0.,0.,0.));
#16457=CARTESIAN_POINT('Origin',(0.,-0.02,0.));
#16458=CARTESIAN_POINT('',(-0.1954,-0.0492,2.39295984553393E-17));
#16459=CARTESIAN_POINT('Origin',(0.,-0.0492,0.));
#16460=CARTESIAN_POINT('',(-0.21,-0.02,-2.57175827820944E-17));
#16461=CARTESIAN_POINT('Origin',(0.,-0.8,0.));
#16462=CARTESIAN_POINT('',(-0.1954,-0.8,-2.39295984553393E-17));
#16463=CARTESIAN_POINT('',(0.,0.,0.));
#16464=CARTESIAN_POINT('',(0.,0.,0.));
#16465=CARTESIAN_POINT('',(0.,0.,0.));
#16466=CARTESIAN_POINT('',(0.,0.,0.));
#16467=CARTESIAN_POINT('',(0.,0.,0.));
#16468=CARTESIAN_POINT('',(0.,0.,0.));
#16469=CARTESIAN_POINT('',(0.,0.,0.));
#16470=CARTESIAN_POINT('',(0.,0.,0.));
#16471=CARTESIAN_POINT('',(0.,0.,0.));
#16472=CARTESIAN_POINT('',(1.76776695296637,1.76776695296637,1.8));
#16473=CARTESIAN_POINT('',(-1.76776695296637,1.76776695296637,1.8));
#16474=CARTESIAN_POINT('',(-1.76776695296637,-1.76776695296637,1.8));
#16475=CARTESIAN_POINT('',(1.76776695296637,-1.76776695296637,1.8));
#16476=CARTESIAN_POINT('',(0.,0.,2.5));
#16477=CARTESIAN_POINT('',(1.23743686707646,1.23743686707646,4.));
#16478=CARTESIAN_POINT('',(-1.23743686707646,1.23743686707646,4.));
#16479=CARTESIAN_POINT('',(-1.23743686707646,-1.23743686707646,4.));
#16480=CARTESIAN_POINT('',(1.23743686707646,-1.23743686707646,4.));
#16481=CARTESIAN_POINT('',(5.,2.,4.));
#16482=CARTESIAN_POINT('',(5.5,0.9,2.));
#16483=CARTESIAN_POINT('',(5.5,3.1,2.));
#16484=CARTESIAN_POINT('',(5.5,2.,5.2));
#16485=CARTESIAN_POINT('',(15.5,0.9,2.));
#16486=CARTESIAN_POINT('',(15.5,3.1,2.));
#16487=CARTESIAN_POINT('',(15.5,2.,5.2));
#16488=CARTESIAN_POINT('',(4.,7.,4.));
#16489=CARTESIAN_POINT('',(2.9,7.5,2.));
#16490=CARTESIAN_POINT('',(5.1,7.5,2.));
#16491=CARTESIAN_POINT('',(4.,7.5,5.2));
#16492=CARTESIAN_POINT('',(2.9,17.5,2.));
#16493=CARTESIAN_POINT('',(5.1,17.5,2.));
#16494=CARTESIAN_POINT('',(4.,17.5,5.2));
#16495=CARTESIAN_POINT('',(0.,0.,0.));
#16496=CARTESIAN_POINT('',(0.,0.,0.));
#16497=CARTESIAN_POINT('',(0.,0.,0.));
#16498=CARTESIAN_POINT('',(0.,0.,0.));
#16499=CARTESIAN_POINT('',(0.,0.,0.));
#16500=CARTESIAN_POINT('',(0.,0.,0.));
#16501=CARTESIAN_POINT('',(0.,0.,0.));
#16502=CARTESIAN_POINT('',(0.,0.,0.));
#16503=CARTESIAN_POINT('',(0.,0.,0.));
#16504=CARTESIAN_POINT('',(0.,0.,0.));
#16505=CARTESIAN_POINT('',(0.,0.,0.));
#16506=CARTESIAN_POINT('',(0.,0.,0.));
#16507=CARTESIAN_POINT('',(-2.5,-2.5,4.8));
#16508=CARTESIAN_POINT('',(0.9,0.,1.4));
#16509=CARTESIAN_POINT('',(0.,2.,10.3));
#16510=CARTESIAN_POINT('',(4.,0.,8.3));
#16511=CARTESIAN_POINT('',(0.,0.,0.));
#16512=CARTESIAN_POINT('',(0.,0.,0.));
#16513=CARTESIAN_POINT('',(0.,0.,0.));
#16514=CARTESIAN_POINT('',(0.,0.,0.));
#16515=CARTESIAN_POINT('',(0.,0.,0.));
#16516=CARTESIAN_POINT('',(0.,0.,0.));
#16517=CARTESIAN_POINT('',(0.,0.,0.));
#16518=CARTESIAN_POINT('',(10.,2.,4.));
#16519=CARTESIAN_POINT('',(8.2,0.8,2.8));
#16520=CARTESIAN_POINT('',(8.2,0.8,5.2));
#16521=CARTESIAN_POINT('',(8.2,3.2,2.8));
#16522=CARTESIAN_POINT('',(8.2,3.2,5.2));
#16523=CARTESIAN_POINT('',(11.8,0.8,2.8));
#16524=CARTESIAN_POINT('',(11.8,0.8,5.2));
#16525=CARTESIAN_POINT('',(11.8,3.2,2.8));
#16526=CARTESIAN_POINT('',(11.8,3.2,5.2));
#16527=CARTESIAN_POINT('',(10.,2.,10.3));
#16528=CARTESIAN_POINT('',(0.,0.,0.));
#16529=CARTESIAN_POINT('',(0.,0.,0.));
#16530=CARTESIAN_POINT('',(0.,0.,0.));
#16531=CARTESIAN_POINT('',(0.,0.,0.));
#16532=CARTESIAN_POINT('',(0.,0.,0.));
#16533=CARTESIAN_POINT('',(0.,0.,0.));
#16534=CARTESIAN_POINT('',(0.,0.,0.));
#16535=CARTESIAN_POINT('',(4.,12.,4.));
#16536=CARTESIAN_POINT('',(2.8,10.2,2.8));
#16537=CARTESIAN_POINT('',(2.8,10.2,5.2));
#16538=CARTESIAN_POINT('',(5.2,10.2,2.8));
#16539=CARTESIAN_POINT('',(5.2,10.2,5.2));
#16540=CARTESIAN_POINT('',(2.8,13.8,2.8));
#16541=CARTESIAN_POINT('',(2.8,13.8,5.2));
#16542=CARTESIAN_POINT('',(5.2,13.8,2.8));
#16543=CARTESIAN_POINT('',(5.2,13.8,5.2));
#16544=CARTESIAN_POINT('',(4.,12.,8.3));
#16545=CARTESIAN_POINT('',(0.,0.,0.));
#16546=CARTESIAN_POINT('',(0.,0.,0.));
#16547=CARTESIAN_POINT('',(0.,0.,0.));
#16548=CARTESIAN_POINT('',(0.,0.,0.));
#16549=CARTESIAN_POINT('',(0.,0.,0.));
#16550=CARTESIAN_POINT('',(0.,0.,0.));
#16551=UNCERTAINTY_MEASURE_WITH_UNIT(LENGTH_MEASURE(0.001),#16679,
'DISTANCE_ACCURACY_VALUE',
'Maximum model space distance between geometric entities at asserted c
onnectivities');
#16552=UNCERTAINTY_MEASURE_WITH_UNIT(LENGTH_MEASURE(0.001),#16679,
'DISTANCE_ACCURACY_VALUE',
'Maximum model space distance between geometric entities at asserted c
onnectivities');
#16553=UNCERTAINTY_MEASURE_WITH_UNIT(LENGTH_MEASURE(0.001),#16679,
'DISTANCE_ACCURACY_VALUE',
'Maximum model space distance between geometric entities at asserted c
onnectivities');
#16554=UNCERTAINTY_MEASURE_WITH_UNIT(LENGTH_MEASURE(0.001),#16679,
'DISTANCE_ACCURACY_VALUE',
'Maximum model space distance between geometric entities at asserted c
onnectivities');
#16555=UNCERTAINTY_MEASURE_WITH_UNIT(LENGTH_MEASURE(0.001),#16679,
'DISTANCE_ACCURACY_VALUE',
'Maximum model space distance between geometric entities at asserted c
onnectivities');
#16556=UNCERTAINTY_MEASURE_WITH_UNIT(LENGTH_MEASURE(0.001),#16679,
'DISTANCE_ACCURACY_VALUE',
'Maximum model space distance between geometric entities at asserted c
onnectivities');
#16557=UNCERTAINTY_MEASURE_WITH_UNIT(LENGTH_MEASURE(0.001),#16679,
'DISTANCE_ACCURACY_VALUE',
'Maximum model space distance between geometric entities at asserted c
onnectivities');
#16558=UNCERTAINTY_MEASURE_WITH_UNIT(LENGTH_MEASURE(0.001),#16679,
'DISTANCE_ACCURACY_VALUE',
'Maximum model space distance between geometric entities at asserted c
onnectivities');
#16559=UNCERTAINTY_MEASURE_WITH_UNIT(LENGTH_MEASURE(0.001),#16679,
'DISTANCE_ACCURACY_VALUE',
'Maximum model space distance between geometric entities at asserted c
onnectivities');
#16560=UNCERTAINTY_MEASURE_WITH_UNIT(LENGTH_MEASURE(0.001),#16679,
'DISTANCE_ACCURACY_VALUE',
'Maximum model space distance between geometric entities at asserted c
onnectivities');
#16561=UNCERTAINTY_MEASURE_WITH_UNIT(LENGTH_MEASURE(0.001),#16679,
'DISTANCE_ACCURACY_VALUE',
'Maximum model space distance between geometric entities at asserted c
onnectivities');
#16562=UNCERTAINTY_MEASURE_WITH_UNIT(LENGTH_MEASURE(0.001),#16679,
'DISTANCE_ACCURACY_VALUE',
'Maximum model space distance between geometric entities at asserted c
onnectivities');
#16563=UNCERTAINTY_MEASURE_WITH_UNIT(LENGTH_MEASURE(0.001),#16679,
'DISTANCE_ACCURACY_VALUE',
'Maximum model space distance between geometric entities at asserted c
onnectivities');
#16564=UNCERTAINTY_MEASURE_WITH_UNIT(LENGTH_MEASURE(0.001),#16679,
'DISTANCE_ACCURACY_VALUE',
'Maximum model space distance between geometric entities at asserted c
onnectivities');
#16565=UNCERTAINTY_MEASURE_WITH_UNIT(LENGTH_MEASURE(0.001),#16679,
'DISTANCE_ACCURACY_VALUE',
'Maximum model space distance between geometric entities at asserted c
onnectivities');
#16566=UNCERTAINTY_MEASURE_WITH_UNIT(LENGTH_MEASURE(0.001),#16679,
'DISTANCE_ACCURACY_VALUE',
'Maximum model space distance between geometric entities at asserted c
onnectivities');
#16567=UNCERTAINTY_MEASURE_WITH_UNIT(LENGTH_MEASURE(0.001),#16679,
'DISTANCE_ACCURACY_VALUE',
'Maximum model space distance between geometric entities at asserted c
onnectivities');
#16568=UNCERTAINTY_MEASURE_WITH_UNIT(LENGTH_MEASURE(0.001),#16679,
'DISTANCE_ACCURACY_VALUE',
'Maximum model space distance between geometric entities at asserted c
onnectivities');
#16569=UNCERTAINTY_MEASURE_WITH_UNIT(LENGTH_MEASURE(0.001),#16679,
'DISTANCE_ACCURACY_VALUE',
'Maximum model space distance between geometric entities at asserted c
onnectivities');
#16570=UNCERTAINTY_MEASURE_WITH_UNIT(LENGTH_MEASURE(0.001),#16679,
'DISTANCE_ACCURACY_VALUE',
'Maximum model space distance between geometric entities at asserted c
onnectivities');
#16571=UNCERTAINTY_MEASURE_WITH_UNIT(LENGTH_MEASURE(0.001),#16679,
'DISTANCE_ACCURACY_VALUE',
'Maximum model space distance between geometric entities at asserted c
onnectivities');
#16572=UNCERTAINTY_MEASURE_WITH_UNIT(LENGTH_MEASURE(0.001),#16679,
'DISTANCE_ACCURACY_VALUE',
'Maximum model space distance between geometric entities at asserted c
onnectivities');
#16573=UNCERTAINTY_MEASURE_WITH_UNIT(LENGTH_MEASURE(0.001),#16679,
'DISTANCE_ACCURACY_VALUE',
'Maximum model space distance between geometric entities at asserted c
onnectivities');
#16574=UNCERTAINTY_MEASURE_WITH_UNIT(LENGTH_MEASURE(0.001),#16679,
'DISTANCE_ACCURACY_VALUE',
'Maximum model space distance between geometric entities at asserted c
onnectivities');
#16575=UNCERTAINTY_MEASURE_WITH_UNIT(LENGTH_MEASURE(0.001),#16679,
'DISTANCE_ACCURACY_VALUE',
'Maximum model space distance between geometric entities at asserted c
onnectivities');
#16576=UNCERTAINTY_MEASURE_WITH_UNIT(LENGTH_MEASURE(0.001),#16679,
'DISTANCE_ACCURACY_VALUE',
'Maximum model space distance between geometric entities at asserted c
onnectivities');
#16577=UNCERTAINTY_MEASURE_WITH_UNIT(LENGTH_MEASURE(0.001),#16679,
'DISTANCE_ACCURACY_VALUE',
'Maximum model space distance between geometric entities at asserted c
onnectivities');
#16578=UNCERTAINTY_MEASURE_WITH_UNIT(LENGTH_MEASURE(0.001),#16679,
'DISTANCE_ACCURACY_VALUE',
'Maximum model space distance between geometric entities at asserted c
onnectivities');
#16579=UNCERTAINTY_MEASURE_WITH_UNIT(LENGTH_MEASURE(0.001),#16679,
'DISTANCE_ACCURACY_VALUE',
'Maximum model space distance between geometric entities at asserted c
onnectivities');
#16580=UNCERTAINTY_MEASURE_WITH_UNIT(LENGTH_MEASURE(0.001),#16679,
'DISTANCE_ACCURACY_VALUE',
'Maximum model space distance between geometric entities at asserted c
onnectivities');
#16581=UNCERTAINTY_MEASURE_WITH_UNIT(LENGTH_MEASURE(0.001),#16679,
'DISTANCE_ACCURACY_VALUE',
'Maximum model space distance between geometric entities at asserted c
onnectivities');
#16582=UNCERTAINTY_MEASURE_WITH_UNIT(LENGTH_MEASURE(0.001),#16679,
'DISTANCE_ACCURACY_VALUE',
'Maximum model space distance between geometric entities at asserted c
onnectivities');
#16583=UNCERTAINTY_MEASURE_WITH_UNIT(LENGTH_MEASURE(0.001),#16679,
'DISTANCE_ACCURACY_VALUE',
'Maximum model space distance between geometric entities at asserted c
onnectivities');
#16584=UNCERTAINTY_MEASURE_WITH_UNIT(LENGTH_MEASURE(0.001),#16679,
'DISTANCE_ACCURACY_VALUE',
'Maximum model space distance between geometric entities at asserted c
onnectivities');
#16585=UNCERTAINTY_MEASURE_WITH_UNIT(LENGTH_MEASURE(0.001),#16679,
'DISTANCE_ACCURACY_VALUE',
'Maximum model space distance between geometric entities at asserted c
onnectivities');
#16586=UNCERTAINTY_MEASURE_WITH_UNIT(LENGTH_MEASURE(0.001),#16679,
'DISTANCE_ACCURACY_VALUE',
'Maximum model space distance between geometric entities at asserted c
onnectivities');
#16587=UNCERTAINTY_MEASURE_WITH_UNIT(LENGTH_MEASURE(0.001),#16679,
'DISTANCE_ACCURACY_VALUE',
'Maximum model space distance between geometric entities at asserted c
onnectivities');
#16588=UNCERTAINTY_MEASURE_WITH_UNIT(LENGTH_MEASURE(0.001),#16679,
'DISTANCE_ACCURACY_VALUE',
'Maximum model space distance between geometric entities at asserted c
onnectivities');
#16589=UNCERTAINTY_MEASURE_WITH_UNIT(LENGTH_MEASURE(0.001),#16679,
'DISTANCE_ACCURACY_VALUE',
'Maximum model space distance between geometric entities at asserted c
onnectivities');
#16590=UNCERTAINTY_MEASURE_WITH_UNIT(LENGTH_MEASURE(0.001),#16679,
'DISTANCE_ACCURACY_VALUE',
'Maximum model space distance between geometric entities at asserted c
onnectivities');
#16591=UNCERTAINTY_MEASURE_WITH_UNIT(LENGTH_MEASURE(0.001),#16679,
'DISTANCE_ACCURACY_VALUE',
'Maximum model space distance between geometric entities at asserted c
onnectivities');
#16592=UNCERTAINTY_MEASURE_WITH_UNIT(LENGTH_MEASURE(0.001),#16679,
'DISTANCE_ACCURACY_VALUE',
'Maximum model space distance between geometric entities at asserted c
onnectivities');
#16593=UNCERTAINTY_MEASURE_WITH_UNIT(LENGTH_MEASURE(0.001),#16679,
'DISTANCE_ACCURACY_VALUE',
'Maximum model space distance between geometric entities at asserted c
onnectivities');
#16594=UNCERTAINTY_MEASURE_WITH_UNIT(LENGTH_MEASURE(0.001),#16679,
'DISTANCE_ACCURACY_VALUE',
'Maximum model space distance between geometric entities at asserted c
onnectivities');
#16595=UNCERTAINTY_MEASURE_WITH_UNIT(LENGTH_MEASURE(0.001),#16679,
'DISTANCE_ACCURACY_VALUE',
'Maximum model space distance between geometric entities at asserted c
onnectivities');
#16596=UNCERTAINTY_MEASURE_WITH_UNIT(LENGTH_MEASURE(0.001),#16679,
'DISTANCE_ACCURACY_VALUE',
'Maximum model space distance between geometric entities at asserted c
onnectivities');
#16597=UNCERTAINTY_MEASURE_WITH_UNIT(LENGTH_MEASURE(0.001),#16679,
'DISTANCE_ACCURACY_VALUE',
'Maximum model space distance between geometric entities at asserted c
onnectivities');
#16598=UNCERTAINTY_MEASURE_WITH_UNIT(LENGTH_MEASURE(0.001),#16679,
'DISTANCE_ACCURACY_VALUE',
'Maximum model space distance between geometric entities at asserted c
onnectivities');
#16599=UNCERTAINTY_MEASURE_WITH_UNIT(LENGTH_MEASURE(0.001),#16679,
'DISTANCE_ACCURACY_VALUE',
'Maximum model space distance between geometric entities at asserted c
onnectivities');
#16600=UNCERTAINTY_MEASURE_WITH_UNIT(LENGTH_MEASURE(0.001),#16679,
'DISTANCE_ACCURACY_VALUE',
'Maximum model space distance between geometric entities at asserted c
onnectivities');
#16601=UNCERTAINTY_MEASURE_WITH_UNIT(LENGTH_MEASURE(0.001),#16679,
'DISTANCE_ACCURACY_VALUE',
'Maximum model space distance between geometric entities at asserted c
onnectivities');
#16602=UNCERTAINTY_MEASURE_WITH_UNIT(LENGTH_MEASURE(0.001),#16679,
'DISTANCE_ACCURACY_VALUE',
'Maximum model space distance between geometric entities at asserted c
onnectivities');
#16603=UNCERTAINTY_MEASURE_WITH_UNIT(LENGTH_MEASURE(0.001),#16679,
'DISTANCE_ACCURACY_VALUE',
'Maximum model space distance between geometric entities at asserted c
onnectivities');
#16604=UNCERTAINTY_MEASURE_WITH_UNIT(LENGTH_MEASURE(0.001),#16679,
'DISTANCE_ACCURACY_VALUE',
'Maximum model space distance between geometric entities at asserted c
onnectivities');
#16605=UNCERTAINTY_MEASURE_WITH_UNIT(LENGTH_MEASURE(0.001),#16679,
'DISTANCE_ACCURACY_VALUE',
'Maximum model space distance between geometric entities at asserted c
onnectivities');
#16606=UNCERTAINTY_MEASURE_WITH_UNIT(LENGTH_MEASURE(0.001),#16679,
'DISTANCE_ACCURACY_VALUE',
'Maximum model space distance between geometric entities at asserted c
onnectivities');
#16607=UNCERTAINTY_MEASURE_WITH_UNIT(LENGTH_MEASURE(0.001),#16679,
'DISTANCE_ACCURACY_VALUE',
'Maximum model space distance between geometric entities at asserted c
onnectivities');
#16608=UNCERTAINTY_MEASURE_WITH_UNIT(LENGTH_MEASURE(0.001),#16679,
'DISTANCE_ACCURACY_VALUE',
'Maximum model space distance between geometric entities at asserted c
onnectivities');
#16609=UNCERTAINTY_MEASURE_WITH_UNIT(LENGTH_MEASURE(0.001),#16679,
'DISTANCE_ACCURACY_VALUE',
'Maximum model space distance between geometric entities at asserted c
onnectivities');
#16610=UNCERTAINTY_MEASURE_WITH_UNIT(LENGTH_MEASURE(0.001),#16679,
'DISTANCE_ACCURACY_VALUE',
'Maximum model space distance between geometric entities at asserted c
onnectivities');
#16611=UNCERTAINTY_MEASURE_WITH_UNIT(LENGTH_MEASURE(0.001),#16679,
'DISTANCE_ACCURACY_VALUE',
'Maximum model space distance between geometric entities at asserted c
onnectivities');
#16612=UNCERTAINTY_MEASURE_WITH_UNIT(LENGTH_MEASURE(0.001),#16679,
'DISTANCE_ACCURACY_VALUE',
'Maximum model space distance between geometric entities at asserted c
onnectivities');
#16613=UNCERTAINTY_MEASURE_WITH_UNIT(LENGTH_MEASURE(0.001),#16679,
'DISTANCE_ACCURACY_VALUE',
'Maximum model space distance between geometric entities at asserted c
onnectivities');
#16614=UNCERTAINTY_MEASURE_WITH_UNIT(LENGTH_MEASURE(0.001),#16679,
'DISTANCE_ACCURACY_VALUE',
'Maximum model space distance between geometric entities at asserted c
onnectivities');
#16615=(
GEOMETRIC_REPRESENTATION_CONTEXT(3)
GLOBAL_UNCERTAINTY_ASSIGNED_CONTEXT((#16551))
GLOBAL_UNIT_ASSIGNED_CONTEXT((#16679,#16681,#16682))
REPRESENTATION_CONTEXT('','3D')
);
#16616=(
GEOMETRIC_REPRESENTATION_CONTEXT(3)
GLOBAL_UNCERTAINTY_ASSIGNED_CONTEXT((#16552))
GLOBAL_UNIT_ASSIGNED_CONTEXT((#16679,#16681,#16682))
REPRESENTATION_CONTEXT('','3D')
);
#16617=(
GEOMETRIC_REPRESENTATION_CONTEXT(3)
GLOBAL_UNCERTAINTY_ASSIGNED_CONTEXT((#16553))
GLOBAL_UNIT_ASSIGNED_CONTEXT((#16679,#16681,#16682))
REPRESENTATION_CONTEXT('','3D')
);
#16618=(
GEOMETRIC_REPRESENTATION_CONTEXT(3)
GLOBAL_UNCERTAINTY_ASSIGNED_CONTEXT((#16554))
GLOBAL_UNIT_ASSIGNED_CONTEXT((#16679,#16681,#16682))
REPRESENTATION_CONTEXT('','3D')
);
#16619=(
GEOMETRIC_REPRESENTATION_CONTEXT(3)
GLOBAL_UNCERTAINTY_ASSIGNED_CONTEXT((#16555))
GLOBAL_UNIT_ASSIGNED_CONTEXT((#16679,#16681,#16682))
REPRESENTATION_CONTEXT('','3D')
);
#16620=(
GEOMETRIC_REPRESENTATION_CONTEXT(3)
GLOBAL_UNCERTAINTY_ASSIGNED_CONTEXT((#16556))
GLOBAL_UNIT_ASSIGNED_CONTEXT((#16679,#16681,#16682))
REPRESENTATION_CONTEXT('','3D')
);
#16621=(
GEOMETRIC_REPRESENTATION_CONTEXT(3)
GLOBAL_UNCERTAINTY_ASSIGNED_CONTEXT((#16557))
GLOBAL_UNIT_ASSIGNED_CONTEXT((#16679,#16681,#16682))
REPRESENTATION_CONTEXT('','3D')
);
#16622=(
GEOMETRIC_REPRESENTATION_CONTEXT(3)
GLOBAL_UNCERTAINTY_ASSIGNED_CONTEXT((#16558))
GLOBAL_UNIT_ASSIGNED_CONTEXT((#16679,#16681,#16682))
REPRESENTATION_CONTEXT('','3D')
);
#16623=(
GEOMETRIC_REPRESENTATION_CONTEXT(3)
GLOBAL_UNCERTAINTY_ASSIGNED_CONTEXT((#16559))
GLOBAL_UNIT_ASSIGNED_CONTEXT((#16679,#16681,#16682))
REPRESENTATION_CONTEXT('','3D')
);
#16624=(
GEOMETRIC_REPRESENTATION_CONTEXT(3)
GLOBAL_UNCERTAINTY_ASSIGNED_CONTEXT((#16560))
GLOBAL_UNIT_ASSIGNED_CONTEXT((#16679,#16681,#16682))
REPRESENTATION_CONTEXT('','3D')
);
#16625=(
GEOMETRIC_REPRESENTATION_CONTEXT(3)
GLOBAL_UNCERTAINTY_ASSIGNED_CONTEXT((#16561))
GLOBAL_UNIT_ASSIGNED_CONTEXT((#16679,#16681,#16682))
REPRESENTATION_CONTEXT('','3D')
);
#16626=(
GEOMETRIC_REPRESENTATION_CONTEXT(3)
GLOBAL_UNCERTAINTY_ASSIGNED_CONTEXT((#16562))
GLOBAL_UNIT_ASSIGNED_CONTEXT((#16679,#16681,#16682))
REPRESENTATION_CONTEXT('','3D')
);
#16627=(
GEOMETRIC_REPRESENTATION_CONTEXT(3)
GLOBAL_UNCERTAINTY_ASSIGNED_CONTEXT((#16563))
GLOBAL_UNIT_ASSIGNED_CONTEXT((#16679,#16681,#16682))
REPRESENTATION_CONTEXT('','3D')
);
#16628=(
GEOMETRIC_REPRESENTATION_CONTEXT(3)
GLOBAL_UNCERTAINTY_ASSIGNED_CONTEXT((#16564))
GLOBAL_UNIT_ASSIGNED_CONTEXT((#16679,#16681,#16682))
REPRESENTATION_CONTEXT('','3D')
);
#16629=(
GEOMETRIC_REPRESENTATION_CONTEXT(3)
GLOBAL_UNCERTAINTY_ASSIGNED_CONTEXT((#16565))
GLOBAL_UNIT_ASSIGNED_CONTEXT((#16679,#16681,#16682))
REPRESENTATION_CONTEXT('','3D')
);
#16630=(
GEOMETRIC_REPRESENTATION_CONTEXT(3)
GLOBAL_UNCERTAINTY_ASSIGNED_CONTEXT((#16566))
GLOBAL_UNIT_ASSIGNED_CONTEXT((#16679,#16681,#16682))
REPRESENTATION_CONTEXT('','3D')
);
#16631=(
GEOMETRIC_REPRESENTATION_CONTEXT(3)
GLOBAL_UNCERTAINTY_ASSIGNED_CONTEXT((#16567))
GLOBAL_UNIT_ASSIGNED_CONTEXT((#16679,#16681,#16682))
REPRESENTATION_CONTEXT('','3D')
);
#16632=(
GEOMETRIC_REPRESENTATION_CONTEXT(3)
GLOBAL_UNCERTAINTY_ASSIGNED_CONTEXT((#16568))
GLOBAL_UNIT_ASSIGNED_CONTEXT((#16679,#16681,#16682))
REPRESENTATION_CONTEXT('','3D')
);
#16633=(
GEOMETRIC_REPRESENTATION_CONTEXT(3)
GLOBAL_UNCERTAINTY_ASSIGNED_CONTEXT((#16569))
GLOBAL_UNIT_ASSIGNED_CONTEXT((#16679,#16681,#16682))
REPRESENTATION_CONTEXT('','3D')
);
#16634=(
GEOMETRIC_REPRESENTATION_CONTEXT(3)
GLOBAL_UNCERTAINTY_ASSIGNED_CONTEXT((#16570))
GLOBAL_UNIT_ASSIGNED_CONTEXT((#16679,#16681,#16682))
REPRESENTATION_CONTEXT('','3D')
);
#16635=(
GEOMETRIC_REPRESENTATION_CONTEXT(3)
GLOBAL_UNCERTAINTY_ASSIGNED_CONTEXT((#16571))
GLOBAL_UNIT_ASSIGNED_CONTEXT((#16679,#16681,#16682))
REPRESENTATION_CONTEXT('','3D')
);
#16636=(
GEOMETRIC_REPRESENTATION_CONTEXT(3)
GLOBAL_UNCERTAINTY_ASSIGNED_CONTEXT((#16572))
GLOBAL_UNIT_ASSIGNED_CONTEXT((#16679,#16681,#16682))
REPRESENTATION_CONTEXT('','3D')
);
#16637=(
GEOMETRIC_REPRESENTATION_CONTEXT(3)
GLOBAL_UNCERTAINTY_ASSIGNED_CONTEXT((#16573))
GLOBAL_UNIT_ASSIGNED_CONTEXT((#16679,#16681,#16682))
REPRESENTATION_CONTEXT('','3D')
);
#16638=(
GEOMETRIC_REPRESENTATION_CONTEXT(3)
GLOBAL_UNCERTAINTY_ASSIGNED_CONTEXT((#16574))
GLOBAL_UNIT_ASSIGNED_CONTEXT((#16679,#16681,#16682))
REPRESENTATION_CONTEXT('','3D')
);
#16639=(
GEOMETRIC_REPRESENTATION_CONTEXT(3)
GLOBAL_UNCERTAINTY_ASSIGNED_CONTEXT((#16575))
GLOBAL_UNIT_ASSIGNED_CONTEXT((#16679,#16681,#16682))
REPRESENTATION_CONTEXT('','3D')
);
#16640=(
GEOMETRIC_REPRESENTATION_CONTEXT(3)
GLOBAL_UNCERTAINTY_ASSIGNED_CONTEXT((#16576))
GLOBAL_UNIT_ASSIGNED_CONTEXT((#16679,#16681,#16682))
REPRESENTATION_CONTEXT('','3D')
);
#16641=(
GEOMETRIC_REPRESENTATION_CONTEXT(3)
GLOBAL_UNCERTAINTY_ASSIGNED_CONTEXT((#16577))
GLOBAL_UNIT_ASSIGNED_CONTEXT((#16679,#16681,#16682))
REPRESENTATION_CONTEXT('','3D')
);
#16642=(
GEOMETRIC_REPRESENTATION_CONTEXT(3)
GLOBAL_UNCERTAINTY_ASSIGNED_CONTEXT((#16578))
GLOBAL_UNIT_ASSIGNED_CONTEXT((#16679,#16681,#16682))
REPRESENTATION_CONTEXT('','3D')
);
#16643=(
GEOMETRIC_REPRESENTATION_CONTEXT(3)
GLOBAL_UNCERTAINTY_ASSIGNED_CONTEXT((#16579))
GLOBAL_UNIT_ASSIGNED_CONTEXT((#16679,#16681,#16682))
REPRESENTATION_CONTEXT('','3D')
);
#16644=(
GEOMETRIC_REPRESENTATION_CONTEXT(3)
GLOBAL_UNCERTAINTY_ASSIGNED_CONTEXT((#16580))
GLOBAL_UNIT_ASSIGNED_CONTEXT((#16679,#16681,#16682))
REPRESENTATION_CONTEXT('','3D')
);
#16645=(
GEOMETRIC_REPRESENTATION_CONTEXT(3)
GLOBAL_UNCERTAINTY_ASSIGNED_CONTEXT((#16581))
GLOBAL_UNIT_ASSIGNED_CONTEXT((#16679,#16681,#16682))
REPRESENTATION_CONTEXT('','3D')
);
#16646=(
GEOMETRIC_REPRESENTATION_CONTEXT(3)
GLOBAL_UNCERTAINTY_ASSIGNED_CONTEXT((#16582))
GLOBAL_UNIT_ASSIGNED_CONTEXT((#16679,#16681,#16682))
REPRESENTATION_CONTEXT('','3D')
);
#16647=(
GEOMETRIC_REPRESENTATION_CONTEXT(3)
GLOBAL_UNCERTAINTY_ASSIGNED_CONTEXT((#16583))
GLOBAL_UNIT_ASSIGNED_CONTEXT((#16679,#16681,#16682))
REPRESENTATION_CONTEXT('','3D')
);
#16648=(
GEOMETRIC_REPRESENTATION_CONTEXT(3)
GLOBAL_UNCERTAINTY_ASSIGNED_CONTEXT((#16584))
GLOBAL_UNIT_ASSIGNED_CONTEXT((#16679,#16681,#16682))
REPRESENTATION_CONTEXT('','3D')
);
#16649=(
GEOMETRIC_REPRESENTATION_CONTEXT(3)
GLOBAL_UNCERTAINTY_ASSIGNED_CONTEXT((#16585))
GLOBAL_UNIT_ASSIGNED_CONTEXT((#16679,#16681,#16682))
REPRESENTATION_CONTEXT('','3D')
);
#16650=(
GEOMETRIC_REPRESENTATION_CONTEXT(3)
GLOBAL_UNCERTAINTY_ASSIGNED_CONTEXT((#16586))
GLOBAL_UNIT_ASSIGNED_CONTEXT((#16679,#16681,#16682))
REPRESENTATION_CONTEXT('','3D')
);
#16651=(
GEOMETRIC_REPRESENTATION_CONTEXT(3)
GLOBAL_UNCERTAINTY_ASSIGNED_CONTEXT((#16587))
GLOBAL_UNIT_ASSIGNED_CONTEXT((#16679,#16681,#16682))
REPRESENTATION_CONTEXT('','3D')
);
#16652=(
GEOMETRIC_REPRESENTATION_CONTEXT(3)
GLOBAL_UNCERTAINTY_ASSIGNED_CONTEXT((#16588))
GLOBAL_UNIT_ASSIGNED_CONTEXT((#16679,#16681,#16682))
REPRESENTATION_CONTEXT('','3D')
);
#16653=(
GEOMETRIC_REPRESENTATION_CONTEXT(3)
GLOBAL_UNCERTAINTY_ASSIGNED_CONTEXT((#16589))
GLOBAL_UNIT_ASSIGNED_CONTEXT((#16679,#16681,#16682))
REPRESENTATION_CONTEXT('','3D')
);
#16654=(
GEOMETRIC_REPRESENTATION_CONTEXT(3)
GLOBAL_UNCERTAINTY_ASSIGNED_CONTEXT((#16590))
GLOBAL_UNIT_ASSIGNED_CONTEXT((#16679,#16681,#16682))
REPRESENTATION_CONTEXT('','3D')
);
#16655=(
GEOMETRIC_REPRESENTATION_CONTEXT(3)
GLOBAL_UNCERTAINTY_ASSIGNED_CONTEXT((#16591))
GLOBAL_UNIT_ASSIGNED_CONTEXT((#16679,#16681,#16682))
REPRESENTATION_CONTEXT('','3D')
);
#16656=(
GEOMETRIC_REPRESENTATION_CONTEXT(3)
GLOBAL_UNCERTAINTY_ASSIGNED_CONTEXT((#16592))
GLOBAL_UNIT_ASSIGNED_CONTEXT((#16679,#16681,#16682))
REPRESENTATION_CONTEXT('','3D')
);
#16657=(
GEOMETRIC_REPRESENTATION_CONTEXT(3)
GLOBAL_UNCERTAINTY_ASSIGNED_CONTEXT((#16593))
GLOBAL_UNIT_ASSIGNED_CONTEXT((#16679,#16681,#16682))
REPRESENTATION_CONTEXT('','3D')
);
#16658=(
GEOMETRIC_REPRESENTATION_CONTEXT(3)
GLOBAL_UNCERTAINTY_ASSIGNED_CONTEXT((#16594))
GLOBAL_UNIT_ASSIGNED_CONTEXT((#16679,#16681,#16682))
REPRESENTATION_CONTEXT('','3D')
);
#16659=(
GEOMETRIC_REPRESENTATION_CONTEXT(3)
GLOBAL_UNCERTAINTY_ASSIGNED_CONTEXT((#16595))
GLOBAL_UNIT_ASSIGNED_CONTEXT((#16679,#16681,#16682))
REPRESENTATION_CONTEXT('','3D')
);
#16660=(
GEOMETRIC_REPRESENTATION_CONTEXT(3)
GLOBAL_UNCERTAINTY_ASSIGNED_CONTEXT((#16596))
GLOBAL_UNIT_ASSIGNED_CONTEXT((#16679,#16681,#16682))
REPRESENTATION_CONTEXT('','3D')
);
#16661=(
GEOMETRIC_REPRESENTATION_CONTEXT(3)
GLOBAL_UNCERTAINTY_ASSIGNED_CONTEXT((#16597))
GLOBAL_UNIT_ASSIGNED_CONTEXT((#16679,#16681,#16682))
REPRESENTATION_CONTEXT('','3D')
);
#16662=(
GEOMETRIC_REPRESENTATION_CONTEXT(3)
GLOBAL_UNCERTAINTY_ASSIGNED_CONTEXT((#16598))
GLOBAL_UNIT_ASSIGNED_CONTEXT((#16679,#16681,#16682))
REPRESENTATION_CONTEXT('','3D')
);
#16663=(
GEOMETRIC_REPRESENTATION_CONTEXT(3)
GLOBAL_UNCERTAINTY_ASSIGNED_CONTEXT((#16599))
GLOBAL_UNIT_ASSIGNED_CONTEXT((#16679,#16681,#16682))
REPRESENTATION_CONTEXT('','3D')
);
#16664=(
GEOMETRIC_REPRESENTATION_CONTEXT(3)
GLOBAL_UNCERTAINTY_ASSIGNED_CONTEXT((#16600))
GLOBAL_UNIT_ASSIGNED_CONTEXT((#16679,#16681,#16682))
REPRESENTATION_CONTEXT('','3D')
);
#16665=(
GEOMETRIC_REPRESENTATION_CONTEXT(3)
GLOBAL_UNCERTAINTY_ASSIGNED_CONTEXT((#16601))
GLOBAL_UNIT_ASSIGNED_CONTEXT((#16679,#16681,#16682))
REPRESENTATION_CONTEXT('','3D')
);
#16666=(
GEOMETRIC_REPRESENTATION_CONTEXT(3)
GLOBAL_UNCERTAINTY_ASSIGNED_CONTEXT((#16602))
GLOBAL_UNIT_ASSIGNED_CONTEXT((#16679,#16681,#16682))
REPRESENTATION_CONTEXT('','3D')
);
#16667=(
GEOMETRIC_REPRESENTATION_CONTEXT(3)
GLOBAL_UNCERTAINTY_ASSIGNED_CONTEXT((#16603))
GLOBAL_UNIT_ASSIGNED_CONTEXT((#16679,#16681,#16682))
REPRESENTATION_CONTEXT('','3D')
);
#16668=(
GEOMETRIC_REPRESENTATION_CONTEXT(3)
GLOBAL_UNCERTAINTY_ASSIGNED_CONTEXT((#16604))
GLOBAL_UNIT_ASSIGNED_CONTEXT((#16679,#16681,#16682))
REPRESENTATION_CONTEXT('','3D')
);
#16669=(
GEOMETRIC_REPRESENTATION_CONTEXT(3)
GLOBAL_UNCERTAINTY_ASSIGNED_CONTEXT((#16605))
GLOBAL_UNIT_ASSIGNED_CONTEXT((#16679,#16681,#16682))
REPRESENTATION_CONTEXT('','3D')
);
#16670=(
GEOMETRIC_REPRESENTATION_CONTEXT(3)
GLOBAL_UNCERTAINTY_ASSIGNED_CONTEXT((#16606))
GLOBAL_UNIT_ASSIGNED_CONTEXT((#16679,#16681,#16682))
REPRESENTATION_CONTEXT('','3D')
);
#16671=(
GEOMETRIC_REPRESENTATION_CONTEXT(3)
GLOBAL_UNCERTAINTY_ASSIGNED_CONTEXT((#16607))
GLOBAL_UNIT_ASSIGNED_CONTEXT((#16679,#16681,#16682))
REPRESENTATION_CONTEXT('','3D')
);
#16672=(
GEOMETRIC_REPRESENTATION_CONTEXT(3)
GLOBAL_UNCERTAINTY_ASSIGNED_CONTEXT((#16608))
GLOBAL_UNIT_ASSIGNED_CONTEXT((#16679,#16681,#16682))
REPRESENTATION_CONTEXT('','3D')
);
#16673=(
GEOMETRIC_REPRESENTATION_CONTEXT(3)
GLOBAL_UNCERTAINTY_ASSIGNED_CONTEXT((#16609))
GLOBAL_UNIT_ASSIGNED_CONTEXT((#16679,#16681,#16682))
REPRESENTATION_CONTEXT('','3D')
);
#16674=(
GEOMETRIC_REPRESENTATION_CONTEXT(3)
GLOBAL_UNCERTAINTY_ASSIGNED_CONTEXT((#16610))
GLOBAL_UNIT_ASSIGNED_CONTEXT((#16679,#16681,#16682))
REPRESENTATION_CONTEXT('','3D')
);
#16675=(
GEOMETRIC_REPRESENTATION_CONTEXT(3)
GLOBAL_UNCERTAINTY_ASSIGNED_CONTEXT((#16611))
GLOBAL_UNIT_ASSIGNED_CONTEXT((#16679,#16681,#16682))
REPRESENTATION_CONTEXT('','3D')
);
#16676=(
GEOMETRIC_REPRESENTATION_CONTEXT(3)
GLOBAL_UNCERTAINTY_ASSIGNED_CONTEXT((#16612))
GLOBAL_UNIT_ASSIGNED_CONTEXT((#16679,#16681,#16682))
REPRESENTATION_CONTEXT('','3D')
);
#16677=(
GEOMETRIC_REPRESENTATION_CONTEXT(3)
GLOBAL_UNCERTAINTY_ASSIGNED_CONTEXT((#16613))
GLOBAL_UNIT_ASSIGNED_CONTEXT((#16679,#16681,#16682))
REPRESENTATION_CONTEXT('','3D')
);
#16678=(
GEOMETRIC_REPRESENTATION_CONTEXT(3)
GLOBAL_UNCERTAINTY_ASSIGNED_CONTEXT((#16614))
GLOBAL_UNIT_ASSIGNED_CONTEXT((#16679,#16681,#16682))
REPRESENTATION_CONTEXT('','3D')
);
#16679=(
LENGTH_UNIT()
NAMED_UNIT(*)
SI_UNIT(.CENTI.,.METRE.)
);
#16680=(
LENGTH_UNIT()
NAMED_UNIT(*)
SI_UNIT($,.METRE.)
);
#16681=(
NAMED_UNIT(*)
PLANE_ANGLE_UNIT()
SI_UNIT($,.RADIAN.)
);
#16682=(
NAMED_UNIT(*)
SI_UNIT($,.STERADIAN.)
SOLID_ANGLE_UNIT()
);
#16683=SHAPE_DEFINITION_REPRESENTATION(#16746,#16910);
#16684=SHAPE_DEFINITION_REPRESENTATION(#16747,#16911);
#16685=SHAPE_DEFINITION_REPRESENTATION(#16748,#16912);
#16686=SHAPE_DEFINITION_REPRESENTATION(#16749,#16913);
#16687=SHAPE_DEFINITION_REPRESENTATION(#16750,#16914);
#16688=SHAPE_DEFINITION_REPRESENTATION(#16751,#16915);
#16689=SHAPE_DEFINITION_REPRESENTATION(#16752,#16916);
#16690=SHAPE_DEFINITION_REPRESENTATION(#16753,#16917);
#16691=SHAPE_DEFINITION_REPRESENTATION(#16754,#16918);
#16692=SHAPE_DEFINITION_REPRESENTATION(#16755,#16919);
#16693=SHAPE_DEFINITION_REPRESENTATION(#16756,#16920);
#16694=SHAPE_DEFINITION_REPRESENTATION(#16757,#16921);
#16695=SHAPE_DEFINITION_REPRESENTATION(#16758,#16922);
#16696=SHAPE_DEFINITION_REPRESENTATION(#16759,#16923);
#16697=SHAPE_DEFINITION_REPRESENTATION(#16760,#16924);
#16698=SHAPE_DEFINITION_REPRESENTATION(#16761,#16925);
#16699=SHAPE_DEFINITION_REPRESENTATION(#16762,#16926);
#16700=SHAPE_DEFINITION_REPRESENTATION(#16763,#16927);
#16701=SHAPE_DEFINITION_REPRESENTATION(#16769,#16928);
#16702=SHAPE_DEFINITION_REPRESENTATION(#16770,#16929);
#16703=SHAPE_DEFINITION_REPRESENTATION(#16771,#16930);
#16704=SHAPE_DEFINITION_REPRESENTATION(#16772,#16931);
#16705=SHAPE_DEFINITION_REPRESENTATION(#16773,#16932);
#16706=SHAPE_DEFINITION_REPRESENTATION(#16774,#16933);
#16707=SHAPE_DEFINITION_REPRESENTATION(#16775,#16934);
#16708=SHAPE_DEFINITION_REPRESENTATION(#16776,#16935);
#16709=SHAPE_DEFINITION_REPRESENTATION(#16777,#16936);
#16710=SHAPE_DEFINITION_REPRESENTATION(#16778,#16937);
#16711=SHAPE_DEFINITION_REPRESENTATION(#16779,#16938);
#16712=SHAPE_DEFINITION_REPRESENTATION(#16780,#16939);
#16713=SHAPE_DEFINITION_REPRESENTATION(#16781,#16940);
#16714=SHAPE_DEFINITION_REPRESENTATION(#16782,#16941);
#16715=SHAPE_DEFINITION_REPRESENTATION(#16783,#16942);
#16716=SHAPE_DEFINITION_REPRESENTATION(#16784,#16943);
#16717=SHAPE_DEFINITION_REPRESENTATION(#16785,#16944);
#16718=SHAPE_DEFINITION_REPRESENTATION(#16786,#16945);
#16719=SHAPE_DEFINITION_REPRESENTATION(#16787,#16946);
#16720=SHAPE_DEFINITION_REPRESENTATION(#16788,#16947);
#16721=SHAPE_DEFINITION_REPRESENTATION(#16789,#16948);
#16722=SHAPE_DEFINITION_REPRESENTATION(#16793,#16949);
#16723=SHAPE_DEFINITION_REPRESENTATION(#16794,#16950);
#16724=SHAPE_DEFINITION_REPRESENTATION(#16795,#16951);
#16725=SHAPE_DEFINITION_REPRESENTATION(#16796,#16952);
#16726=SHAPE_DEFINITION_REPRESENTATION(#16800,#16953);
#16727=SHAPE_DEFINITION_REPRESENTATION(#16801,#16954);
#16728=SHAPE_DEFINITION_REPRESENTATION(#16802,#16955);
#16729=SHAPE_DEFINITION_REPRESENTATION(#16803,#16956);
#16730=SHAPE_DEFINITION_REPRESENTATION(#16804,#16957);
#16731=SHAPE_DEFINITION_REPRESENTATION(#16805,#16958);
#16732=SHAPE_DEFINITION_REPRESENTATION(#16806,#16959);
#16733=SHAPE_DEFINITION_REPRESENTATION(#16807,#16960);
#16734=SHAPE_DEFINITION_REPRESENTATION(#16808,#16961);
#16735=SHAPE_DEFINITION_REPRESENTATION(#16809,#16962);
#16736=SHAPE_DEFINITION_REPRESENTATION(#16810,#16963);
#16737=SHAPE_DEFINITION_REPRESENTATION(#16811,#16964);
#16738=SHAPE_DEFINITION_REPRESENTATION(#16812,#16965);
#16739=SHAPE_DEFINITION_REPRESENTATION(#16813,#16966);
#16740=SHAPE_DEFINITION_REPRESENTATION(#16814,#16967);
#16741=SHAPE_DEFINITION_REPRESENTATION(#16815,#16968);
#16742=SHAPE_DEFINITION_REPRESENTATION(#16816,#16969);
#16743=SHAPE_DEFINITION_REPRESENTATION(#16817,#16970);
#16744=SHAPE_DEFINITION_REPRESENTATION(#16818,#16971);
#16745=SHAPE_DEFINITION_REPRESENTATION(#16821,#16972);
#16746=PRODUCT_DEFINITION_SHAPE('',$,#16974);
#16747=PRODUCT_DEFINITION_SHAPE('',$,#16975);
#16748=PRODUCT_DEFINITION_SHAPE('',$,#16976);
#16749=PRODUCT_DEFINITION_SHAPE('',$,#16977);
#16750=PRODUCT_DEFINITION_SHAPE('',$,#16978);
#16751=PRODUCT_DEFINITION_SHAPE('',$,#16979);
#16752=PRODUCT_DEFINITION_SHAPE('',$,#16980);
#16753=PRODUCT_DEFINITION_SHAPE('',$,#16981);
#16754=PRODUCT_DEFINITION_SHAPE('',$,#16982);
#16755=PRODUCT_DEFINITION_SHAPE('',$,#16983);
#16756=PRODUCT_DEFINITION_SHAPE('',$,#16984);
#16757=PRODUCT_DEFINITION_SHAPE('',$,#16985);
#16758=PRODUCT_DEFINITION_SHAPE('',$,#16986);
#16759=PRODUCT_DEFINITION_SHAPE('',$,#16987);
#16760=PRODUCT_DEFINITION_SHAPE('',$,#16988);
#16761=PRODUCT_DEFINITION_SHAPE('',$,#16989);
#16762=PRODUCT_DEFINITION_SHAPE('',$,#16990);
#16763=PRODUCT_DEFINITION_SHAPE('',$,#16991);
#16764=PRODUCT_DEFINITION_SHAPE($,$,#314);
#16765=PRODUCT_DEFINITION_SHAPE($,$,#315);
#16766=PRODUCT_DEFINITION_SHAPE($,$,#316);
#16767=PRODUCT_DEFINITION_SHAPE($,$,#317);
#16768=PRODUCT_DEFINITION_SHAPE($,$,#318);
#16769=PRODUCT_DEFINITION_SHAPE('',$,#16992);
#16770=PRODUCT_DEFINITION_SHAPE('',$,#16993);
#16771=PRODUCT_DEFINITION_SHAPE('',$,#16994);
#16772=PRODUCT_DEFINITION_SHAPE('',$,#16995);
#16773=PRODUCT_DEFINITION_SHAPE('',$,#16996);
#16774=PRODUCT_DEFINITION_SHAPE('',$,#16997);
#16775=PRODUCT_DEFINITION_SHAPE('',$,#16998);
#16776=PRODUCT_DEFINITION_SHAPE('',$,#16999);
#16777=PRODUCT_DEFINITION_SHAPE('',$,#17000);
#16778=PRODUCT_DEFINITION_SHAPE('',$,#17001);
#16779=PRODUCT_DEFINITION_SHAPE('',$,#17002);
#16780=PRODUCT_DEFINITION_SHAPE('',$,#17003);
#16781=PRODUCT_DEFINITION_SHAPE('',$,#17004);
#16782=PRODUCT_DEFINITION_SHAPE('',$,#17005);
#16783=PRODUCT_DEFINITION_SHAPE('',$,#17006);
#16784=PRODUCT_DEFINITION_SHAPE('',$,#17007);
#16785=PRODUCT_DEFINITION_SHAPE('',$,#17008);
#16786=PRODUCT_DEFINITION_SHAPE('',$,#17009);
#16787=PRODUCT_DEFINITION_SHAPE('',$,#17010);
#16788=PRODUCT_DEFINITION_SHAPE('',$,#17011);
#16789=PRODUCT_DEFINITION_SHAPE('',$,#17012);
#16790=PRODUCT_DEFINITION_SHAPE($,$,#319);
#16791=PRODUCT_DEFINITION_SHAPE($,$,#320);
#16792=PRODUCT_DEFINITION_SHAPE($,$,#321);
#16793=PRODUCT_DEFINITION_SHAPE('',$,#17013);
#16794=PRODUCT_DEFINITION_SHAPE('',$,#17014);
#16795=PRODUCT_DEFINITION_SHAPE('',$,#17015);
#16796=PRODUCT_DEFINITION_SHAPE('',$,#17016);
#16797=PRODUCT_DEFINITION_SHAPE($,$,#322);
#16798=PRODUCT_DEFINITION_SHAPE($,$,#323);
#16799=PRODUCT_DEFINITION_SHAPE($,$,#324);
#16800=PRODUCT_DEFINITION_SHAPE('',$,#17017);
#16801=PRODUCT_DEFINITION_SHAPE('',$,#17018);
#16802=PRODUCT_DEFINITION_SHAPE('',$,#17019);
#16803=PRODUCT_DEFINITION_SHAPE('',$,#17020);
#16804=PRODUCT_DEFINITION_SHAPE('',$,#17021);
#16805=PRODUCT_DEFINITION_SHAPE('',$,#17022);
#16806=PRODUCT_DEFINITION_SHAPE('',$,#17023);
#16807=PRODUCT_DEFINITION_SHAPE('',$,#17024);
#16808=PRODUCT_DEFINITION_SHAPE('',$,#17025);
#16809=PRODUCT_DEFINITION_SHAPE('',$,#17026);
#16810=PRODUCT_DEFINITION_SHAPE('',$,#17027);
#16811=PRODUCT_DEFINITION_SHAPE('',$,#17028);
#16812=PRODUCT_DEFINITION_SHAPE('',$,#17029);
#16813=PRODUCT_DEFINITION_SHAPE('',$,#17030);
#16814=PRODUCT_DEFINITION_SHAPE('',$,#17031);
#16815=PRODUCT_DEFINITION_SHAPE('',$,#17032);
#16816=PRODUCT_DEFINITION_SHAPE('',$,#17033);
#16817=PRODUCT_DEFINITION_SHAPE('',$,#17034);
#16818=PRODUCT_DEFINITION_SHAPE('',$,#17035);
#16819=PRODUCT_DEFINITION_SHAPE($,$,#325);
#16820=PRODUCT_DEFINITION_SHAPE($,$,#326);
#16821=PRODUCT_DEFINITION_SHAPE('',$,#17036);
#16822=PRODUCT_DEFINITION_SHAPE($,$,#327);
#16823=PRODUCT_DEFINITION_SHAPE($,$,#328);
#16824=PRODUCT_DEFINITION_SHAPE($,$,#329);
#16825=PRODUCT_DEFINITION_SHAPE($,$,#330);
#16826=PRODUCT_DEFINITION_SHAPE($,$,#331);
#16827=PRODUCT_DEFINITION_SHAPE($,$,#332);
#16828=PRODUCT_DEFINITION_SHAPE($,$,#333);
#16829=PRODUCT_DEFINITION_SHAPE($,$,#334);
#16830=PRODUCT_DEFINITION_SHAPE($,$,#335);
#16831=PRODUCT_DEFINITION_SHAPE($,$,#336);
#16832=PRODUCT_DEFINITION_SHAPE($,$,#337);
#16833=PRODUCT_DEFINITION_SHAPE($,$,#338);
#16834=PRODUCT_DEFINITION_SHAPE($,$,#339);
#16835=PRODUCT_DEFINITION_SHAPE($,$,#340);
#16836=PRODUCT_DEFINITION_SHAPE($,$,#341);
#16837=PRODUCT_DEFINITION_SHAPE($,$,#342);
#16838=PRODUCT_DEFINITION_SHAPE($,$,#343);
#16839=PRODUCT_DEFINITION_SHAPE($,$,#344);
#16840=PRODUCT_DEFINITION_SHAPE($,$,#345);
#16841=PRODUCT_DEFINITION_SHAPE($,$,#346);
#16842=PRODUCT_DEFINITION_SHAPE($,$,#347);
#16843=PRODUCT_DEFINITION_SHAPE($,$,#348);
#16844=PRODUCT_DEFINITION_SHAPE($,$,#349);
#16845=PRODUCT_DEFINITION_SHAPE($,$,#350);
#16846=PRODUCT_DEFINITION_SHAPE($,$,#351);
#16847=PRODUCT_DEFINITION_SHAPE($,$,#352);
#16848=PRODUCT_DEFINITION_SHAPE($,$,#353);
#16849=PRODUCT_DEFINITION_SHAPE($,$,#354);
#16850=PRODUCT_DEFINITION_SHAPE($,$,#355);
#16851=PRODUCT_DEFINITION_SHAPE($,$,#356);
#16852=PRODUCT_DEFINITION_SHAPE($,$,#357);
#16853=PRODUCT_DEFINITION_SHAPE($,$,#358);
#16854=PRODUCT_DEFINITION_SHAPE($,$,#359);
#16855=PRODUCT_DEFINITION_SHAPE($,$,#360);
#16856=PRODUCT_DEFINITION_SHAPE($,$,#361);
#16857=PRODUCT_DEFINITION_SHAPE($,$,#362);
#16858=PRODUCT_DEFINITION_SHAPE($,$,#363);
#16859=PRODUCT_DEFINITION_SHAPE($,$,#364);
#16860=PRODUCT_DEFINITION_SHAPE($,$,#365);
#16861=PRODUCT_DEFINITION_SHAPE($,$,#366);
#16862=PRODUCT_DEFINITION_SHAPE($,$,#367);
#16863=PRODUCT_DEFINITION_SHAPE($,$,#368);
#16864=PRODUCT_DEFINITION_SHAPE($,$,#369);
#16865=PRODUCT_DEFINITION_SHAPE($,$,#370);
#16866=PRODUCT_DEFINITION_SHAPE($,$,#371);
#16867=PRODUCT_DEFINITION_SHAPE($,$,#372);
#16868=PRODUCT_DEFINITION_SHAPE($,$,#373);
#16869=PRODUCT_DEFINITION_SHAPE($,$,#374);
#16870=PRODUCT_DEFINITION_SHAPE($,$,#375);
#16871=PRODUCT_DEFINITION_SHAPE($,$,#376);
#16872=PRODUCT_DEFINITION_SHAPE($,$,#377);
#16873=PRODUCT_DEFINITION_SHAPE($,$,#378);
#16874=PRODUCT_DEFINITION_SHAPE($,$,#379);
#16875=PRODUCT_DEFINITION_SHAPE($,$,#380);
#16876=PRODUCT_DEFINITION_SHAPE($,$,#381);
#16877=PRODUCT_DEFINITION_SHAPE($,$,#382);
#16878=PRODUCT_DEFINITION_SHAPE($,$,#383);
#16879=PRODUCT_DEFINITION_SHAPE($,$,#384);
#16880=PRODUCT_DEFINITION_SHAPE($,$,#385);
#16881=PRODUCT_DEFINITION_SHAPE($,$,#386);
#16882=PRODUCT_DEFINITION_SHAPE($,$,#387);
#16883=PRODUCT_DEFINITION_SHAPE($,$,#388);
#16884=PRODUCT_DEFINITION_SHAPE($,$,#389);
#16885=PRODUCT_DEFINITION_SHAPE($,$,#390);
#16886=PRODUCT_DEFINITION_SHAPE($,$,#391);
#16887=PRODUCT_DEFINITION_SHAPE($,$,#392);
#16888=PRODUCT_DEFINITION_SHAPE($,$,#393);
#16889=PRODUCT_DEFINITION_SHAPE($,$,#394);
#16890=PRODUCT_DEFINITION_SHAPE($,$,#395);
#16891=PRODUCT_DEFINITION_SHAPE($,$,#396);
#16892=PRODUCT_DEFINITION_SHAPE($,$,#397);
#16893=PRODUCT_DEFINITION_SHAPE($,$,#398);
#16894=PRODUCT_DEFINITION_SHAPE($,$,#399);
#16895=PRODUCT_DEFINITION_SHAPE($,$,#400);
#16896=PRODUCT_DEFINITION_SHAPE($,$,#401);
#16897=PRODUCT_DEFINITION_SHAPE($,$,#402);
#16898=PRODUCT_DEFINITION_SHAPE($,$,#403);
#16899=PRODUCT_DEFINITION_SHAPE($,$,#404);
#16900=PRODUCT_DEFINITION_SHAPE($,$,#405);
#16901=PRODUCT_DEFINITION_SHAPE($,$,#406);
#16902=PRODUCT_DEFINITION_SHAPE($,$,#407);
#16903=PRODUCT_DEFINITION_SHAPE($,$,#408);
#16904=PRODUCT_DEFINITION_SHAPE($,$,#409);
#16905=PRODUCT_DEFINITION_SHAPE($,$,#410);
#16906=PRODUCT_DEFINITION_SHAPE($,$,#411);
#16907=PRODUCT_DEFINITION_SHAPE($,$,#412);
#16908=PRODUCT_DEFINITION_SHAPE($,$,#413);
#16909=PRODUCT_DEFINITION_SHAPE($,$,#414);
#16910=SHAPE_REPRESENTATION('',(#9454,#10624,#10625,#10626,#10627,#10628,
#10629),#16615);
#16911=SHAPE_REPRESENTATION('',(#9455,#10542,#10543,#10544,#10545,#10546,
#10547,#10548,#10549,#10550,#10551,#10552,#10553,#10554,#10555,#10556,#10557,
#10558,#10559,#10560,#10561,#10562,#10563,#10564,#10565,#10566,#10567,#10568,
#10569,#10570,#10571,#10572,#10573),#16616);
#16912=SHAPE_REPRESENTATION('',(#9456),#16617);
#16913=SHAPE_REPRESENTATION('',(#9499),#16618);
#16914=SHAPE_REPRESENTATION('',(#9506),#16619);
#16915=SHAPE_REPRESENTATION('',(#9513),#16620);
#16916=SHAPE_REPRESENTATION('',(#9583),#16621);
#16917=SHAPE_REPRESENTATION('',(#9624),#16622);
#16918=SHAPE_REPRESENTATION('',(#9660),#16623);
#16919=SHAPE_REPRESENTATION('',(#9696),#16624);
#16920=SHAPE_REPRESENTATION('',(#9730),#16625);
#16921=SHAPE_REPRESENTATION('',(#9764),#16626);
#16922=SHAPE_REPRESENTATION('',(#9788,#9917,#9918,#9919,#9920,#9921),#16627);
#16923=SHAPE_REPRESENTATION('',(#9789),#16628);
#16924=SHAPE_REPRESENTATION('',(#9809),#16629);
#16925=SHAPE_REPRESENTATION('',(#9829),#16630);
#16926=SHAPE_REPRESENTATION('',(#9846),#16631);
#16927=SHAPE_REPRESENTATION('',(#9900),#16632);
#16928=SHAPE_REPRESENTATION('',(#9922),#16633);
#16929=SHAPE_REPRESENTATION('',(#9930),#16634);
#16930=SHAPE_REPRESENTATION('',(#9947,#10574,#10575,#10576,#10577,#10578,
#10579,#10580,#10581,#10582,#10583,#10584,#10585,#10586,#10587,#10588,#10589),
#16635);
#16931=SHAPE_REPRESENTATION('',(#9948),#16636);
#16932=SHAPE_REPRESENTATION('',(#9992),#16637);
#16933=SHAPE_REPRESENTATION('',(#10002),#16638);
#16934=SHAPE_REPRESENTATION('',(#10011),#16639);
#16935=SHAPE_REPRESENTATION('',(#10025),#16640);
#16936=SHAPE_REPRESENTATION('',(#10043),#16641);
#16937=SHAPE_REPRESENTATION('',(#10052),#16642);
#16938=SHAPE_REPRESENTATION('',(#10061),#16643);
#16939=SHAPE_REPRESENTATION('',(#10070),#16644);
#16940=SHAPE_REPRESENTATION('',(#10088),#16645);
#16941=SHAPE_REPRESENTATION('',(#10097),#16646);
#16942=SHAPE_REPRESENTATION('',(#10106),#16647);
#16943=SHAPE_REPRESENTATION('',(#10115),#16648);
#16944=SHAPE_REPRESENTATION('',(#10141),#16649);
#16945=SHAPE_REPRESENTATION('',(#10156,#10192,#10193,#10194),#16650);
#16946=SHAPE_REPRESENTATION('',(#10157),#16651);
#16947=SHAPE_REPRESENTATION('',(#10174),#16652);
#16948=SHAPE_REPRESENTATION('',(#10183),#16653);
#16949=SHAPE_REPRESENTATION('',(#10195,#10231,#10232,#10233),#16654);
#16950=SHAPE_REPRESENTATION('',(#10196),#16655);
#16951=SHAPE_REPRESENTATION('',(#10213),#16656);
#16952=SHAPE_REPRESENTATION('',(#10222),#16657);
#16953=SHAPE_REPRESENTATION('',(#10234,#10590,#10591,#10592,#10593,#10594,
#10595,#10596,#10597,#10598,#10599,#10600,#10601,#10602,#10603,#10604,#10605,
#10606),#16658);
#16954=SHAPE_REPRESENTATION('',(#10235),#16659);
#16955=SHAPE_REPRESENTATION('',(#10261),#16660);
#16956=SHAPE_REPRESENTATION('',(#10283),#16661);
#16957=SHAPE_REPRESENTATION('',(#10305),#16662);
#16958=SHAPE_REPRESENTATION('',(#10323),#16663);
#16959=SHAPE_REPRESENTATION('',(#10332),#16664);
#16960=SHAPE_REPRESENTATION('',(#10341),#16665);
#16961=SHAPE_REPRESENTATION('',(#10350,#10607,#10608,#10609,#10610,#10611,
#10612,#10613,#10614,#10615,#10616,#10617,#10618,#10619,#10620,#10621,#10622,
#10623),#16666);
#16962=SHAPE_REPRESENTATION('',(#10351),#16667);
#16963=SHAPE_REPRESENTATION('',(#10377),#16668);
#16964=SHAPE_REPRESENTATION('',(#10399),#16669);
#16965=SHAPE_REPRESENTATION('',(#10421),#16670);
#16966=SHAPE_REPRESENTATION('',(#10439),#16671);
#16967=SHAPE_REPRESENTATION('',(#10448),#16672);
#16968=SHAPE_REPRESENTATION('',(#10457),#16673);
#16969=SHAPE_REPRESENTATION('',(#10466,#10516,#10517),#16674);
#16970=SHAPE_REPRESENTATION('',(#10467),#16675);
#16971=SHAPE_REPRESENTATION('',(#10499),#16676);
#16972=SHAPE_REPRESENTATION('',(#10518),#16677);
#16973=PRODUCT_DEFINITION_CONTEXT('part definition',#17164,'design');
#16974=PRODUCT_DEFINITION('PAT-009',
'PAT-009',#17037,#16973);
#16975=PRODUCT_DEFINITION('Frame and linear guides',
'Frame and linear guides',#17038,#16973);
#16976=PRODUCT_DEFINITION('Base','Base',#17039,#16973);
#16977=PRODUCT_DEFINITION('Foot strip','Foot strip',#17040,#16973);
#16978=PRODUCT_DEFINITION('Foot strip (1)','Foot strip (1)',#17041,#16973);
#16979=PRODUCT_DEFINITION('Pivot pedestal','Pivot pedestal',#17042,#16973);
#16980=PRODUCT_DEFINITION('Pivot cap','Pivot cap',#17043,#16973);
#16981=PRODUCT_DEFINITION('Horizontal shaft support',
'Horizontal shaft support',#17044,#16973);
#16982=PRODUCT_DEFINITION('Horizontal shaft support (1)',
'Horizontal shaft support (1)',#17045,#16973);
#16983=PRODUCT_DEFINITION('Vertical shaft support',
'Vertical shaft support',#17046,#16973);
#16984=PRODUCT_DEFINITION('Vertical shaft support (1)',
'Vertical shaft support (1)',#17047,#16973);
#16985=PRODUCT_DEFINITION('M5x14 Cap Screw','M5x14 Cap Screw',#17048,#16973);
#16986=PRODUCT_DEFINITION('Sealed Ball Bearing - 10 x 30 x 9 mm',
'Sealed Ball Bearing - 10 x 30 x 9 mm',#17049,#16973);
#16987=PRODUCT_DEFINITION('Inner ring','Inner ring',#17050,#16973);
#16988=PRODUCT_DEFINITION('Outer ring','Outer ring',#17051,#16973);
#16989=PRODUCT_DEFINITION('Balls','Balls',#17052,#16973);
#16990=PRODUCT_DEFINITION('Cage','Cage',#17053,#16973);
#16991=PRODUCT_DEFINITION('Seals 2RS','Seals 2RS',#17054,#16973);
#16992=PRODUCT_DEFINITION('Guide shaft 110 mm','Guide shaft 110 mm',#17055,
#16973);
#16993=PRODUCT_DEFINITION('Socket Set Screw - M4x6',
'Socket Set Screw - M4x6',#17056,#16973);
#16994=PRODUCT_DEFINITION('Bell crank and spindle',
'Bell crank and spindle',#17057,#16973);
#16995=PRODUCT_DEFINITION('Bell crank and spindle (1)',
'Bell crank and spindle (1)',#17058,#16973);
#16996=PRODUCT_DEFINITION('Input grip','Input grip',#17059,#16973);
#16997=PRODUCT_DEFINITION('Lower race sleeve','Lower race sleeve',#17060,
#16973);
#16998=PRODUCT_DEFINITION('Spindle collar','Spindle collar',#17061,#16973);
#16999=PRODUCT_DEFINITION('Horizontal link pin','Horizontal link pin',#17062,
#16973);
#17000=PRODUCT_DEFINITION('Horizontal lower pin sleeve',
'Horizontal lower pin sleeve',#17063,#16973);
#17001=PRODUCT_DEFINITION('Upper pin sleeve','Upper pin sleeve',#17064,
#16973);
#17002=PRODUCT_DEFINITION('Pin keeper','Pin keeper',#17065,#16973);
#17003=PRODUCT_DEFINITION('Vertical link pin','Vertical link pin',#17066,
#16973);
#17004=PRODUCT_DEFINITION('Vertical lower pin sleeve',
'Vertical lower pin sleeve',#17067,#16973);
#17005=PRODUCT_DEFINITION('Upper pin sleeve (1)','Upper pin sleeve (1)',#17068,
#16973);
#17006=PRODUCT_DEFINITION('Pin keeper (1)','Pin keeper (1)',#17069,#16973);
#17007=PRODUCT_DEFINITION('Cap Screw - M4x16','Cap Screw - M4x16',#17070,
#16973);
#17008=PRODUCT_DEFINITION('M4x4 collar screw','M4x4 collar screw',#17071,
#16973);
#17009=PRODUCT_DEFINITION('Short-arm connecting rod',
'Short-arm connecting rod',#17072,#16973);
#17010=PRODUCT_DEFINITION('Horizontal connecting link',
'Horizontal connecting link',#17073,#16973);
#17011=PRODUCT_DEFINITION('Plain link bushing','Plain link bushing',#17074,
#16973);
#17012=PRODUCT_DEFINITION('Plain link bushing (1)',
'Plain link bushing (1)',#17075,#16973);
#17013=PRODUCT_DEFINITION('Long-arm connecting rod',
'Long-arm connecting rod',#17076,#16973);
#17014=PRODUCT_DEFINITION('Vertical connecting link',
'Vertical connecting link',#17077,#16973);
#17015=PRODUCT_DEFINITION('Plain link bushing (2)',
'Plain link bushing (2)',#17078,#16973);
#17016=PRODUCT_DEFINITION('Plain link bushing (3)',
'Plain link bushing (3)',#17079,#16973);
#17017=PRODUCT_DEFINITION('Horizontal output carriage',
'Horizontal output carriage',#17080,#16973);
#17018=PRODUCT_DEFINITION('Horizontal output housing',
'Horizontal output housing',#17081,#16973);
#17019=PRODUCT_DEFINITION('Horizontal guide cap','Horizontal guide cap',
#17082,#16973);
#17020=PRODUCT_DEFINITION('Horizontal guide cap (1)',
'Horizontal guide cap (1)',#17083,#16973);
#17021=PRODUCT_DEFINITION('Horizontal link pin (1)',
'Horizontal link pin (1)',#17084,#16973);
#17022=PRODUCT_DEFINITION('Horizontal lower pin sleeve (1)',
'Horizontal lower pin sleeve (1)',#17085,#16973);
#17023=PRODUCT_DEFINITION('Upper pin sleeve (2)','Upper pin sleeve (2)',#17086,
#16973);
#17024=PRODUCT_DEFINITION('Pin keeper (2)','Pin keeper (2)',#17087,#16973);
#17025=PRODUCT_DEFINITION('Vertical output carriage',
'Vertical output carriage',#17088,#16973);
#17026=PRODUCT_DEFINITION('Vertical output housing',
'Vertical output housing',#17089,#16973);
#17027=PRODUCT_DEFINITION('Vertical guide cap','Vertical guide cap',#17090,
#16973);
#17028=PRODUCT_DEFINITION('Vertical guide cap (1)',
'Vertical guide cap (1)',#17091,#16973);
#17029=PRODUCT_DEFINITION('Vertical link pin (1)','Vertical link pin (1)',
#17092,#16973);
#17030=PRODUCT_DEFINITION('Vertical lower pin sleeve (1)',
'Vertical lower pin sleeve (1)',#17093,#16973);
#17031=PRODUCT_DEFINITION('Upper pin sleeve (3)','Upper pin sleeve (3)',#17094,
#16973);
#17032=PRODUCT_DEFINITION('Pin keeper (3)','Pin keeper (3)',#17095,#16973);
#17033=PRODUCT_DEFINITION('Linear Ball Bushing - 12 x 21 x 30 mm',
'Linear Ball Bushing - 12 x 21 x 30 mm',#17096,#16973);
#17034=PRODUCT_DEFINITION('Steel sleeve','Steel sleeve',#17097,#16973);
#17035=PRODUCT_DEFINITION('Ball retainer (plastic)',
'Ball retainer (plastic)',#17098,#16973);
#17036=PRODUCT_DEFINITION('M4x10 Cap Screw','M4x10 Cap Screw',#17099,#16973);
#17037=PRODUCT_DEFINITION_FORMATION('',$,#17166);
#17038=PRODUCT_DEFINITION_FORMATION('',$,#17167);
#17039=PRODUCT_DEFINITION_FORMATION('',$,#17168);
#17040=PRODUCT_DEFINITION_FORMATION('',$,#17169);
#17041=PRODUCT_DEFINITION_FORMATION('',$,#17170);
#17042=PRODUCT_DEFINITION_FORMATION('',$,#17171);
#17043=PRODUCT_DEFINITION_FORMATION('',$,#17172);
#17044=PRODUCT_DEFINITION_FORMATION('',$,#17173);
#17045=PRODUCT_DEFINITION_FORMATION('',$,#17174);
#17046=PRODUCT_DEFINITION_FORMATION('',$,#17175);
#17047=PRODUCT_DEFINITION_FORMATION('',$,#17176);
#17048=PRODUCT_DEFINITION_FORMATION('',$,#17177);
#17049=PRODUCT_DEFINITION_FORMATION('',$,#17178);
#17050=PRODUCT_DEFINITION_FORMATION('',$,#17179);
#17051=PRODUCT_DEFINITION_FORMATION('',$,#17180);
#17052=PRODUCT_DEFINITION_FORMATION('',$,#17181);
#17053=PRODUCT_DEFINITION_FORMATION('',$,#17182);
#17054=PRODUCT_DEFINITION_FORMATION('',$,#17183);
#17055=PRODUCT_DEFINITION_FORMATION('',$,#17184);
#17056=PRODUCT_DEFINITION_FORMATION('',$,#17185);
#17057=PRODUCT_DEFINITION_FORMATION('',$,#17186);
#17058=PRODUCT_DEFINITION_FORMATION('',$,#17187);
#17059=PRODUCT_DEFINITION_FORMATION('',$,#17188);
#17060=PRODUCT_DEFINITION_FORMATION('',$,#17189);
#17061=PRODUCT_DEFINITION_FORMATION('',$,#17190);
#17062=PRODUCT_DEFINITION_FORMATION('',$,#17191);
#17063=PRODUCT_DEFINITION_FORMATION('',$,#17192);
#17064=PRODUCT_DEFINITION_FORMATION('',$,#17193);
#17065=PRODUCT_DEFINITION_FORMATION('',$,#17194);
#17066=PRODUCT_DEFINITION_FORMATION('',$,#17195);
#17067=PRODUCT_DEFINITION_FORMATION('',$,#17196);
#17068=PRODUCT_DEFINITION_FORMATION('',$,#17197);
#17069=PRODUCT_DEFINITION_FORMATION('',$,#17198);
#17070=PRODUCT_DEFINITION_FORMATION('',$,#17199);
#17071=PRODUCT_DEFINITION_FORMATION('',$,#17200);
#17072=PRODUCT_DEFINITION_FORMATION('',$,#17201);
#17073=PRODUCT_DEFINITION_FORMATION('',$,#17202);
#17074=PRODUCT_DEFINITION_FORMATION('',$,#17203);
#17075=PRODUCT_DEFINITION_FORMATION('',$,#17204);
#17076=PRODUCT_DEFINITION_FORMATION('',$,#17205);
#17077=PRODUCT_DEFINITION_FORMATION('',$,#17206);
#17078=PRODUCT_DEFINITION_FORMATION('',$,#17207);
#17079=PRODUCT_DEFINITION_FORMATION('',$,#17208);
#17080=PRODUCT_DEFINITION_FORMATION('',$,#17209);
#17081=PRODUCT_DEFINITION_FORMATION('',$,#17210);
#17082=PRODUCT_DEFINITION_FORMATION('',$,#17211);
#17083=PRODUCT_DEFINITION_FORMATION('',$,#17212);
#17084=PRODUCT_DEFINITION_FORMATION('',$,#17213);
#17085=PRODUCT_DEFINITION_FORMATION('',$,#17214);
#17086=PRODUCT_DEFINITION_FORMATION('',$,#17215);
#17087=PRODUCT_DEFINITION_FORMATION('',$,#17216);
#17088=PRODUCT_DEFINITION_FORMATION('',$,#17217);
#17089=PRODUCT_DEFINITION_FORMATION('',$,#17218);
#17090=PRODUCT_DEFINITION_FORMATION('',$,#17219);
#17091=PRODUCT_DEFINITION_FORMATION('',$,#17220);
#17092=PRODUCT_DEFINITION_FORMATION('',$,#17221);
#17093=PRODUCT_DEFINITION_FORMATION('',$,#17222);
#17094=PRODUCT_DEFINITION_FORMATION('',$,#17223);
#17095=PRODUCT_DEFINITION_FORMATION('',$,#17224);
#17096=PRODUCT_DEFINITION_FORMATION('',$,#17225);
#17097=PRODUCT_DEFINITION_FORMATION('',$,#17226);
#17098=PRODUCT_DEFINITION_FORMATION('',$,#17227);
#17099=PRODUCT_DEFINITION_FORMATION('',$,#17228);
#17100=PRODUCT_RELATED_PRODUCT_CATEGORY('PAT-009','PAT-009',(#17166));
#17101=PRODUCT_RELATED_PRODUCT_CATEGORY('Frame and linear guides',
'Frame and linear guides',(#17167));
#17102=PRODUCT_RELATED_PRODUCT_CATEGORY('Base','Base',(#17168));
#17103=PRODUCT_RELATED_PRODUCT_CATEGORY('Foot strip','Foot strip',(#17169));
#17104=PRODUCT_RELATED_PRODUCT_CATEGORY('Foot strip (1)',
'Foot strip (1)',(#17170));
#17105=PRODUCT_RELATED_PRODUCT_CATEGORY('Pivot pedestal',
'Pivot pedestal',(#17171));
#17106=PRODUCT_RELATED_PRODUCT_CATEGORY('Pivot cap','Pivot cap',(#17172));
#17107=PRODUCT_RELATED_PRODUCT_CATEGORY('Horizontal shaft support',
'Horizontal shaft support',(#17173));
#17108=PRODUCT_RELATED_PRODUCT_CATEGORY('Horizontal shaft support (1)',
'Horizontal shaft support (1)',(#17174));
#17109=PRODUCT_RELATED_PRODUCT_CATEGORY('Vertical shaft support',
'Vertical shaft support',(#17175));
#17110=PRODUCT_RELATED_PRODUCT_CATEGORY('Vertical shaft support (1)',
'Vertical shaft support (1)',(#17176));
#17111=PRODUCT_RELATED_PRODUCT_CATEGORY('M5x14 Cap Screw',
'M5x14 Cap Screw',(#17177));
#17112=PRODUCT_RELATED_PRODUCT_CATEGORY(
'Sealed Ball Bearing - 10 x 30 x 9 mm',
'Sealed Ball Bearing - 10 x 30 x 9 mm',(#17178));
#17113=PRODUCT_RELATED_PRODUCT_CATEGORY('Inner ring','Inner ring',(#17179));
#17114=PRODUCT_RELATED_PRODUCT_CATEGORY('Outer ring','Outer ring',(#17180));
#17115=PRODUCT_RELATED_PRODUCT_CATEGORY('Balls','Balls',(#17181));
#17116=PRODUCT_RELATED_PRODUCT_CATEGORY('Cage','Cage',(#17182));
#17117=PRODUCT_RELATED_PRODUCT_CATEGORY('Seals 2RS','Seals 2RS',(#17183));
#17118=PRODUCT_RELATED_PRODUCT_CATEGORY('Guide shaft 110 mm',
'Guide shaft 110 mm',(#17184));
#17119=PRODUCT_RELATED_PRODUCT_CATEGORY('Socket Set Screw - M4x6',
'Socket Set Screw - M4x6',(#17185));
#17120=PRODUCT_RELATED_PRODUCT_CATEGORY('Bell crank and spindle',
'Bell crank and spindle',(#17186));
#17121=PRODUCT_RELATED_PRODUCT_CATEGORY('Bell crank and spindle (1)',
'Bell crank and spindle (1)',(#17187));
#17122=PRODUCT_RELATED_PRODUCT_CATEGORY('Input grip','Input grip',(#17188));
#17123=PRODUCT_RELATED_PRODUCT_CATEGORY('Lower race sleeve',
'Lower race sleeve',(#17189));
#17124=PRODUCT_RELATED_PRODUCT_CATEGORY('Spindle collar',
'Spindle collar',(#17190));
#17125=PRODUCT_RELATED_PRODUCT_CATEGORY('Horizontal link pin',
'Horizontal link pin',(#17191));
#17126=PRODUCT_RELATED_PRODUCT_CATEGORY('Horizontal lower pin sleeve',
'Horizontal lower pin sleeve',(#17192));
#17127=PRODUCT_RELATED_PRODUCT_CATEGORY('Upper pin sleeve',
'Upper pin sleeve',(#17193));
#17128=PRODUCT_RELATED_PRODUCT_CATEGORY('Pin keeper','Pin keeper',(#17194));
#17129=PRODUCT_RELATED_PRODUCT_CATEGORY('Vertical link pin',
'Vertical link pin',(#17195));
#17130=PRODUCT_RELATED_PRODUCT_CATEGORY('Vertical lower pin sleeve',
'Vertical lower pin sleeve',(#17196));
#17131=PRODUCT_RELATED_PRODUCT_CATEGORY('Upper pin sleeve (1)',
'Upper pin sleeve (1)',(#17197));
#17132=PRODUCT_RELATED_PRODUCT_CATEGORY('Pin keeper (1)',
'Pin keeper (1)',(#17198));
#17133=PRODUCT_RELATED_PRODUCT_CATEGORY('Cap Screw - M4x16',
'Cap Screw - M4x16',(#17199));
#17134=PRODUCT_RELATED_PRODUCT_CATEGORY('M4x4 collar screw',
'M4x4 collar screw',(#17200));
#17135=PRODUCT_RELATED_PRODUCT_CATEGORY('Short-arm connecting rod',
'Short-arm connecting rod',(#17201));
#17136=PRODUCT_RELATED_PRODUCT_CATEGORY('Horizontal connecting link',
'Horizontal connecting link',(#17202));
#17137=PRODUCT_RELATED_PRODUCT_CATEGORY('Plain link bushing',
'Plain link bushing',(#17203));
#17138=PRODUCT_RELATED_PRODUCT_CATEGORY('Plain link bushing (1)',
'Plain link bushing (1)',(#17204));
#17139=PRODUCT_RELATED_PRODUCT_CATEGORY('Long-arm connecting rod',
'Long-arm connecting rod',(#17205));
#17140=PRODUCT_RELATED_PRODUCT_CATEGORY('Vertical connecting link',
'Vertical connecting link',(#17206));
#17141=PRODUCT_RELATED_PRODUCT_CATEGORY('Plain link bushing (2)',
'Plain link bushing (2)',(#17207));
#17142=PRODUCT_RELATED_PRODUCT_CATEGORY('Plain link bushing (3)',
'Plain link bushing (3)',(#17208));
#17143=PRODUCT_RELATED_PRODUCT_CATEGORY('Horizontal output carriage',
'Horizontal output carriage',(#17209));
#17144=PRODUCT_RELATED_PRODUCT_CATEGORY('Horizontal output housing',
'Horizontal output housing',(#17210));
#17145=PRODUCT_RELATED_PRODUCT_CATEGORY('Horizontal guide cap',
'Horizontal guide cap',(#17211));
#17146=PRODUCT_RELATED_PRODUCT_CATEGORY('Horizontal guide cap (1)',
'Horizontal guide cap (1)',(#17212));
#17147=PRODUCT_RELATED_PRODUCT_CATEGORY('Horizontal link pin (1)',
'Horizontal link pin (1)',(#17213));
#17148=PRODUCT_RELATED_PRODUCT_CATEGORY(
'Horizontal lower pin sleeve (1)','Horizontal lower pin sleeve (1)',(#17214));
#17149=PRODUCT_RELATED_PRODUCT_CATEGORY('Upper pin sleeve (2)',
'Upper pin sleeve (2)',(#17215));
#17150=PRODUCT_RELATED_PRODUCT_CATEGORY('Pin keeper (2)',
'Pin keeper (2)',(#17216));
#17151=PRODUCT_RELATED_PRODUCT_CATEGORY('Vertical output carriage',
'Vertical output carriage',(#17217));
#17152=PRODUCT_RELATED_PRODUCT_CATEGORY('Vertical output housing',
'Vertical output housing',(#17218));
#17153=PRODUCT_RELATED_PRODUCT_CATEGORY('Vertical guide cap',
'Vertical guide cap',(#17219));
#17154=PRODUCT_RELATED_PRODUCT_CATEGORY('Vertical guide cap (1)',
'Vertical guide cap (1)',(#17220));
#17155=PRODUCT_RELATED_PRODUCT_CATEGORY('Vertical link pin (1)',
'Vertical link pin (1)',(#17221));
#17156=PRODUCT_RELATED_PRODUCT_CATEGORY('Vertical lower pin sleeve (1)',
'Vertical lower pin sleeve (1)',(#17222));
#17157=PRODUCT_RELATED_PRODUCT_CATEGORY('Upper pin sleeve (3)',
'Upper pin sleeve (3)',(#17223));
#17158=PRODUCT_RELATED_PRODUCT_CATEGORY('Pin keeper (3)',
'Pin keeper (3)',(#17224));
#17159=PRODUCT_RELATED_PRODUCT_CATEGORY(
'Linear Ball Bushing - 12 x 21 x 30 mm',
'Linear Ball Bushing - 12 x 21 x 30 mm',(#17225));
#17160=PRODUCT_RELATED_PRODUCT_CATEGORY('Steel sleeve','Steel sleeve',(#17226));
#17161=PRODUCT_RELATED_PRODUCT_CATEGORY('Ball retainer (plastic)',
'Ball retainer (plastic)',(#17227));
#17162=PRODUCT_RELATED_PRODUCT_CATEGORY('M4x10 Cap Screw',
'M4x10 Cap Screw',(#17228));
#17163=APPLICATION_PROTOCOL_DEFINITION('international standard',
'automotive_design',2009,#17164);
#17164=APPLICATION_CONTEXT(
'Core Data for Automotive Mechanical Design Process');
#17165=PRODUCT_CONTEXT('part definition',#17164,'mechanical');
#17166=PRODUCT('PAT-009','PAT-009',
'PAT-009',(#17165));
#17167=PRODUCT('Frame and linear guides','Frame and linear guides',
'Frame and linear guides',(#17165));
#17168=PRODUCT('Base','Base','Base',(#17165));
#17169=PRODUCT('Foot strip','Foot strip','Foot strip',(#17165));
#17170=PRODUCT('Foot strip (1)','Foot strip (1)','Foot strip (1)',(#17165));
#17171=PRODUCT('Pivot pedestal','Pivot pedestal','Pivot pedestal',(#17165));
#17172=PRODUCT('Pivot cap','Pivot cap','Pivot cap',(#17165));
#17173=PRODUCT('Horizontal shaft support','Horizontal shaft support',
'Horizontal shaft support',(#17165));
#17174=PRODUCT('Horizontal shaft support (1)',
'Horizontal shaft support (1)','Horizontal shaft support (1)',(#17165));
#17175=PRODUCT('Vertical shaft support','Vertical shaft support',
'Vertical shaft support',(#17165));
#17176=PRODUCT('Vertical shaft support (1)','Vertical shaft support (1)',
'Vertical shaft support (1)',(#17165));
#17177=PRODUCT('M5x14 Cap Screw','M5x14 Cap Screw','M5x14 Cap Screw',(#17165));
#17178=PRODUCT('Sealed Ball Bearing - 10 x 30 x 9 mm',
'Sealed Ball Bearing - 10 x 30 x 9 mm',
'Sealed Ball Bearing - 10 x 30 x 9 mm',(#17165));
#17179=PRODUCT('Inner ring','Inner ring','Inner ring',(#17165));
#17180=PRODUCT('Outer ring','Outer ring','Outer ring',(#17165));
#17181=PRODUCT('Balls','Balls','Balls',(#17165));
#17182=PRODUCT('Cage','Cage','Cage',(#17165));
#17183=PRODUCT('Seals 2RS','Seals 2RS','Seals 2RS',(#17165));
#17184=PRODUCT('Guide shaft 110 mm','Guide shaft 110 mm',
'Guide shaft 110 mm',(#17165));
#17185=PRODUCT('Socket Set Screw - M4x6','Socket Set Screw - M4x6',
'Socket Set Screw - M4x6',(#17165));
#17186=PRODUCT('Bell crank and spindle','Bell crank and spindle',
'Bell crank and spindle',(#17165));
#17187=PRODUCT('Bell crank and spindle (1)','Bell crank and spindle (1)',
'Bell crank and spindle (1)',(#17165));
#17188=PRODUCT('Input grip','Input grip','Input grip',(#17165));
#17189=PRODUCT('Lower race sleeve','Lower race sleeve',
'Lower race sleeve',(#17165));
#17190=PRODUCT('Spindle collar','Spindle collar','Spindle collar',(#17165));
#17191=PRODUCT('Horizontal link pin','Horizontal link pin',
'Horizontal link pin',(#17165));
#17192=PRODUCT('Horizontal lower pin sleeve',
'Horizontal lower pin sleeve','Horizontal lower pin sleeve',(#17165));
#17193=PRODUCT('Upper pin sleeve','Upper pin sleeve','Upper pin sleeve',
(#17165));
#17194=PRODUCT('Pin keeper','Pin keeper','Pin keeper',(#17165));
#17195=PRODUCT('Vertical link pin','Vertical link pin',
'Vertical link pin',(#17165));
#17196=PRODUCT('Vertical lower pin sleeve','Vertical lower pin sleeve',
'Vertical lower pin sleeve',(#17165));
#17197=PRODUCT('Upper pin sleeve (1)','Upper pin sleeve (1)',
'Upper pin sleeve (1)',(#17165));
#17198=PRODUCT('Pin keeper (1)','Pin keeper (1)','Pin keeper (1)',(#17165));
#17199=PRODUCT('Cap Screw - M4x16','Cap Screw - M4x16',
'Cap Screw - M4x16',(#17165));
#17200=PRODUCT('M4x4 collar screw','M4x4 collar screw',
'M4x4 collar screw',(#17165));
#17201=PRODUCT('Short-arm connecting rod','Short-arm connecting rod',
'Short-arm connecting rod',(#17165));
#17202=PRODUCT('Horizontal connecting link',
'Horizontal connecting link','Horizontal connecting link',(#17165));
#17203=PRODUCT('Plain link bushing','Plain link bushing',
'Plain link bushing',(#17165));
#17204=PRODUCT('Plain link bushing (1)','Plain link bushing (1)',
'Plain link bushing (1)',(#17165));
#17205=PRODUCT('Long-arm connecting rod','Long-arm connecting rod',
'Long-arm connecting rod',(#17165));
#17206=PRODUCT('Vertical connecting link','Vertical connecting link',
'Vertical connecting link',(#17165));
#17207=PRODUCT('Plain link bushing (2)','Plain link bushing (2)',
'Plain link bushing (2)',(#17165));
#17208=PRODUCT('Plain link bushing (3)','Plain link bushing (3)',
'Plain link bushing (3)',(#17165));
#17209=PRODUCT('Horizontal output carriage',
'Horizontal output carriage','Horizontal output carriage',(#17165));
#17210=PRODUCT('Horizontal output housing','Horizontal output housing',
'Horizontal output housing',(#17165));
#17211=PRODUCT('Horizontal guide cap','Horizontal guide cap',
'Horizontal guide cap',(#17165));
#17212=PRODUCT('Horizontal guide cap (1)','Horizontal guide cap (1)',
'Horizontal guide cap (1)',(#17165));
#17213=PRODUCT('Horizontal link pin (1)','Horizontal link pin (1)',
'Horizontal link pin (1)',(#17165));
#17214=PRODUCT('Horizontal lower pin sleeve (1)',
'Horizontal lower pin sleeve (1)','Horizontal lower pin sleeve (1)',(#17165));
#17215=PRODUCT('Upper pin sleeve (2)','Upper pin sleeve (2)',
'Upper pin sleeve (2)',(#17165));
#17216=PRODUCT('Pin keeper (2)','Pin keeper (2)','Pin keeper (2)',(#17165));
#17217=PRODUCT('Vertical output carriage','Vertical output carriage',
'Vertical output carriage',(#17165));
#17218=PRODUCT('Vertical output housing','Vertical output housing',
'Vertical output housing',(#17165));
#17219=PRODUCT('Vertical guide cap','Vertical guide cap',
'Vertical guide cap',(#17165));
#17220=PRODUCT('Vertical guide cap (1)','Vertical guide cap (1)',
'Vertical guide cap (1)',(#17165));
#17221=PRODUCT('Vertical link pin (1)','Vertical link pin (1)',
'Vertical link pin (1)',(#17165));
#17222=PRODUCT('Vertical lower pin sleeve (1)',
'Vertical lower pin sleeve (1)','Vertical lower pin sleeve (1)',(#17165));
#17223=PRODUCT('Upper pin sleeve (3)','Upper pin sleeve (3)',
'Upper pin sleeve (3)',(#17165));
#17224=PRODUCT('Pin keeper (3)','Pin keeper (3)','Pin keeper (3)',(#17165));
#17225=PRODUCT('Linear Ball Bushing - 12 x 21 x 30 mm',
'Linear Ball Bushing - 12 x 21 x 30 mm',
'Linear Ball Bushing - 12 x 21 x 30 mm',(#17165));
#17226=PRODUCT('Steel sleeve','Steel sleeve','Steel sleeve',(#17165));
#17227=PRODUCT('Ball retainer (plastic)','Ball retainer (plastic)',
'Ball retainer (plastic)',(#17165));
#17228=PRODUCT('M4x10 Cap Screw','M4x10 Cap Screw','M4x10 Cap Screw',(#17165));
#17229=PRESENTATION_STYLE_ASSIGNMENT((#17234));
#17230=PRESENTATION_STYLE_ASSIGNMENT((#17235));
#17231=PRESENTATION_STYLE_ASSIGNMENT((#17236));
#17232=PRESENTATION_STYLE_ASSIGNMENT((#17237));
#17233=PRESENTATION_STYLE_ASSIGNMENT((#17238));
#17234=SURFACE_STYLE_USAGE(.BOTH.,#17239);
#17235=SURFACE_STYLE_USAGE(.BOTH.,#17240);
#17236=SURFACE_STYLE_USAGE(.BOTH.,#17241);
#17237=SURFACE_STYLE_USAGE(.BOTH.,#17242);
#17238=SURFACE_STYLE_USAGE(.BOTH.,#17243);
#17239=SURFACE_SIDE_STYLE('',(#17244));
#17240=SURFACE_SIDE_STYLE('',(#17245));
#17241=SURFACE_SIDE_STYLE('',(#17246));
#17242=SURFACE_SIDE_STYLE('',(#17247));
#17243=SURFACE_SIDE_STYLE('',(#17248));
#17244=SURFACE_STYLE_FILL_AREA(#17249);
#17245=SURFACE_STYLE_FILL_AREA(#17250);
#17246=SURFACE_STYLE_FILL_AREA(#17251);
#17247=SURFACE_STYLE_FILL_AREA(#17252);
#17248=SURFACE_STYLE_FILL_AREA(#17253);
#17249=FILL_AREA_STYLE('Steel - Satin',(#17254));
#17250=FILL_AREA_STYLE('CAD Library Painted - Deep blue',(#17255));
#17251=FILL_AREA_STYLE('CAD Library Painted - Engineering blue',(#17256));
#17252=FILL_AREA_STYLE('CAD Library Painted - Steel gray',(#17257));
#17253=FILL_AREA_STYLE('CAD Library Painted - Graphite',(#17258));
#17254=FILL_AREA_STYLE_COLOUR('Steel - Satin',#17259);
#17255=FILL_AREA_STYLE_COLOUR('CAD Library Painted - Deep blue',#17260);
#17256=FILL_AREA_STYLE_COLOUR('CAD Library Painted - Engineering blue',
#17261);
#17257=FILL_AREA_STYLE_COLOUR('CAD Library Painted - Steel gray',#17262);
#17258=FILL_AREA_STYLE_COLOUR('CAD Library Painted - Graphite',#17263);
#17259=COLOUR_RGB('Steel - Satin',0.627450980392157,0.627450980392157,0.627450980392157);
#17260=COLOUR_RGB('CAD Library Painted - Deep blue',0.0784313725490196,
0.203921568627451,0.349019607843137);
#17261=COLOUR_RGB('CAD Library Painted - Engineering blue',0.12156862745098,
0.356862745098039,0.6);
#17262=COLOUR_RGB('CAD Library Painted - Steel gray',0.592156862745098,
0.631372549019608,0.67843137254902);
#17263=COLOUR_RGB('CAD Library Painted - Graphite',0.168627450980392,0.192156862745098,
0.231372549019608);
#17264=COLOUR_RGB('Dark Blue',0.08,0.2,0.34);
#17265=FILL_AREA_STYLE_COLOUR('',#17264);
#17266=FILL_AREA_STYLE('',(#17265));
#17267=SURFACE_STYLE_FILL_AREA(#17266);
#17268=SURFACE_SIDE_STYLE('',(#17267));
#17269=SURFACE_STYLE_USAGE(.BOTH.,#17268);
#17270=PRESENTATION_STYLE_ASSIGNMENT((#17269));
#17271=COLOUR_RGB('Light Blue',0.38,0.62,0.78);
#17272=FILL_AREA_STYLE_COLOUR('',#17271);
#17273=FILL_AREA_STYLE('',(#17272));
#17274=SURFACE_STYLE_FILL_AREA(#17273);
#17275=SURFACE_SIDE_STYLE('',(#17274));
#17276=SURFACE_STYLE_USAGE(.BOTH.,#17275);
#17277=PRESENTATION_STYLE_ASSIGNMENT((#17276));
#17278=COLOUR_RGB('Sky Blue',0.24,0.69,0.87);
#17279=FILL_AREA_STYLE_COLOUR('',#17278);
#17280=FILL_AREA_STYLE('',(#17279));
#17281=SURFACE_STYLE_FILL_AREA(#17280);
#17282=SURFACE_SIDE_STYLE('',(#17281));
#17283=SURFACE_STYLE_USAGE(.BOTH.,#17282);
#17284=PRESENTATION_STYLE_ASSIGNMENT((#17283));
#17285=COLOUR_RGB('Grey',0.48,0.52,0.57);
#17286=FILL_AREA_STYLE_COLOUR('',#17285);
#17287=FILL_AREA_STYLE('',(#17286));
#17288=SURFACE_STYLE_FILL_AREA(#17287);
#17289=SURFACE_SIDE_STYLE('',(#17288));
#17290=SURFACE_STYLE_USAGE(.BOTH.,#17289);
#17291=PRESENTATION_STYLE_ASSIGNMENT((#17290));
#17292=COLOUR_RGB('Black',0.12,0.14,0.17);
#17293=FILL_AREA_STYLE_COLOUR('',#17292);
#17294=FILL_AREA_STYLE('',(#17293));
#17295=SURFACE_STYLE_FILL_AREA(#17294);
#17296=SURFACE_SIDE_STYLE('',(#17295));
#17297=SURFACE_STYLE_USAGE(.BOTH.,#17296);
#17298=PRESENTATION_STYLE_ASSIGNMENT((#17297));
#17299=COLOUR_RGB('Off White',0.89,0.88,0.83);
#17300=FILL_AREA_STYLE_COLOUR('',#17299);
#17301=FILL_AREA_STYLE('',(#17300));
#17302=SURFACE_STYLE_FILL_AREA(#17301);
#17303=SURFACE_SIDE_STYLE('',(#17302));
#17304=SURFACE_STYLE_USAGE(.BOTH.,#17303);
#17305=PRESENTATION_STYLE_ASSIGNMENT((#17304));
ENDSEC;
END-ISO-10303-21;
